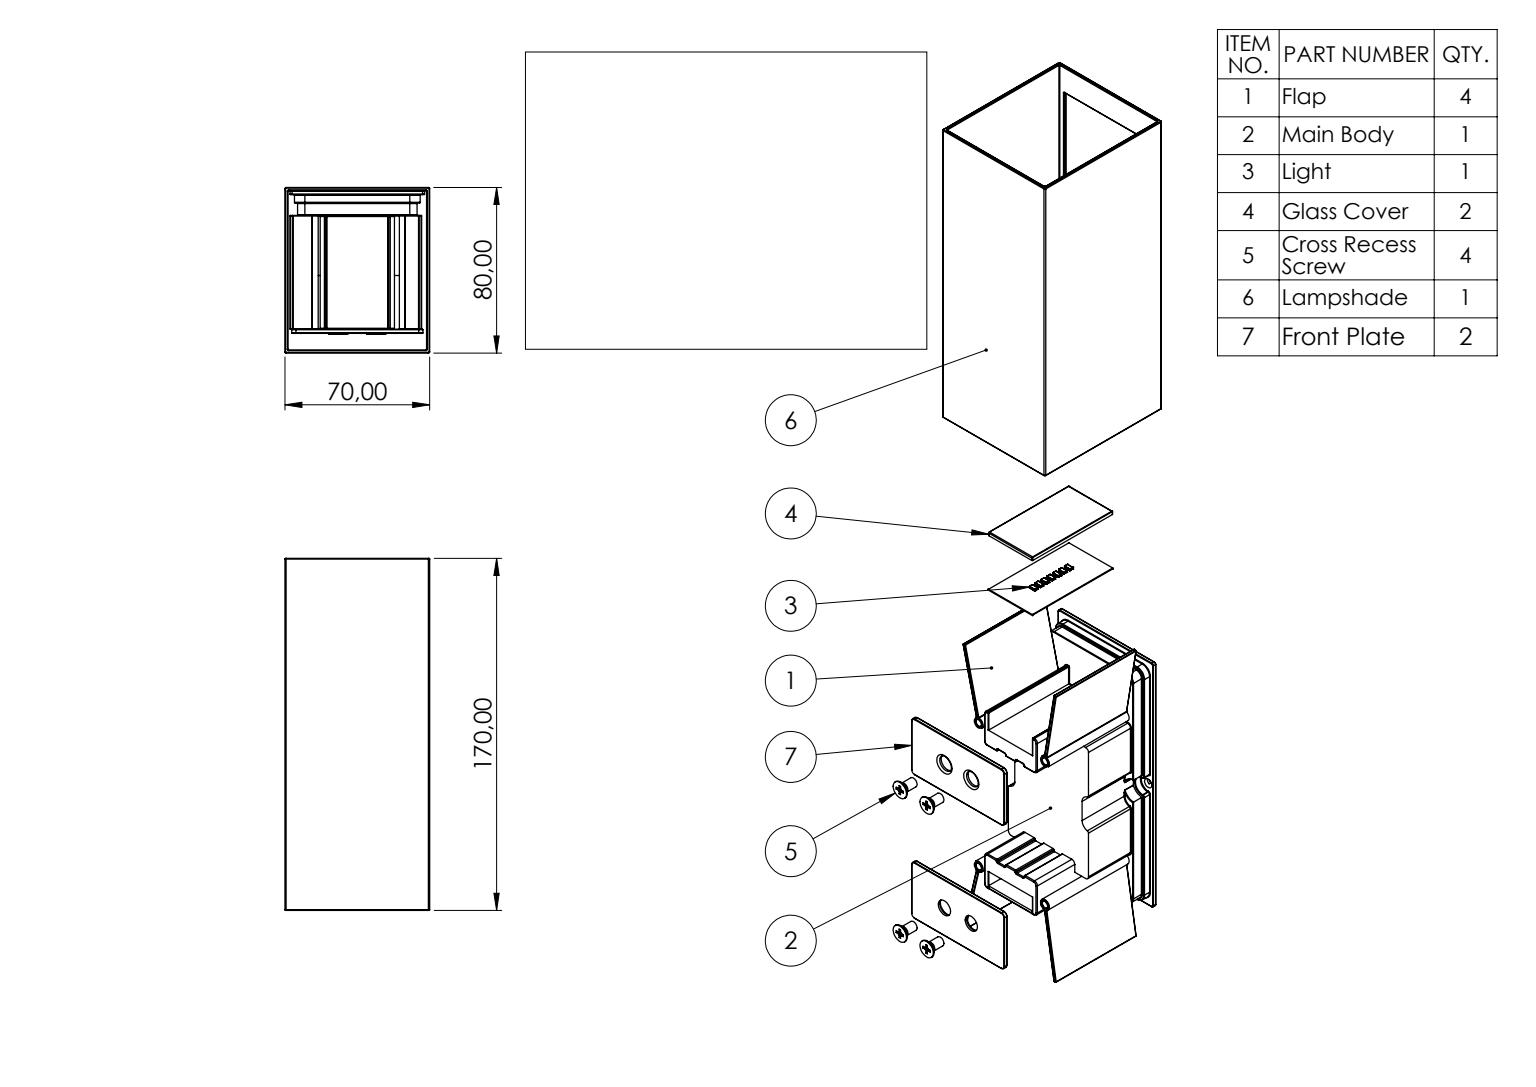
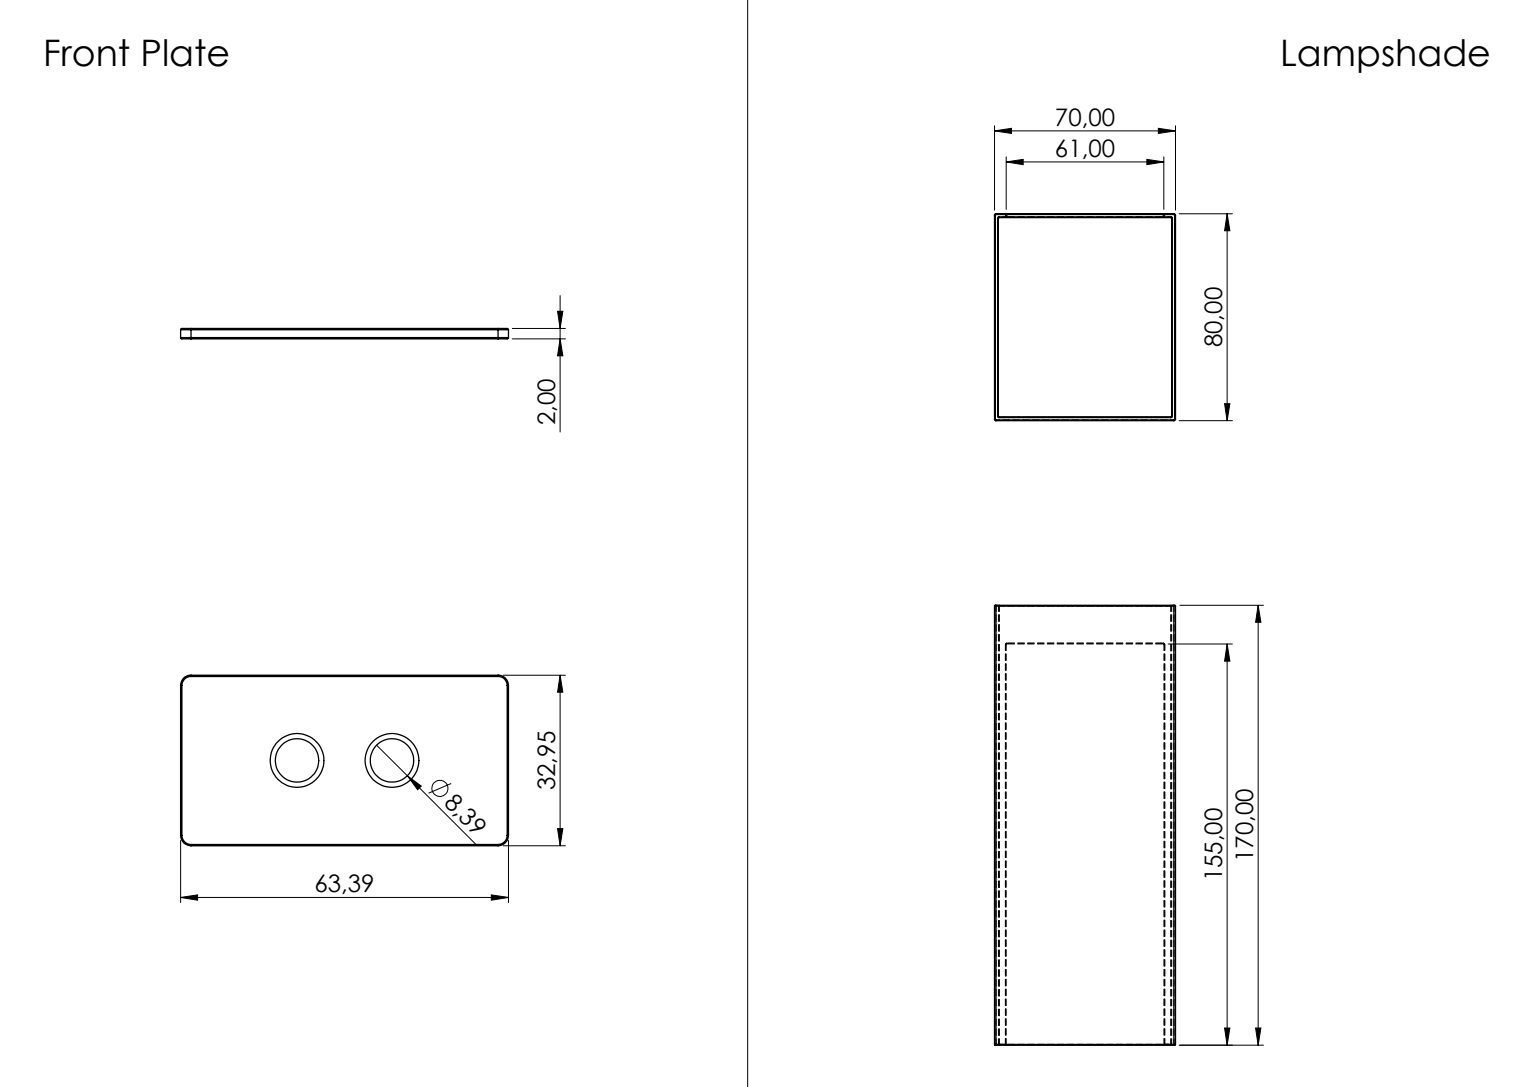
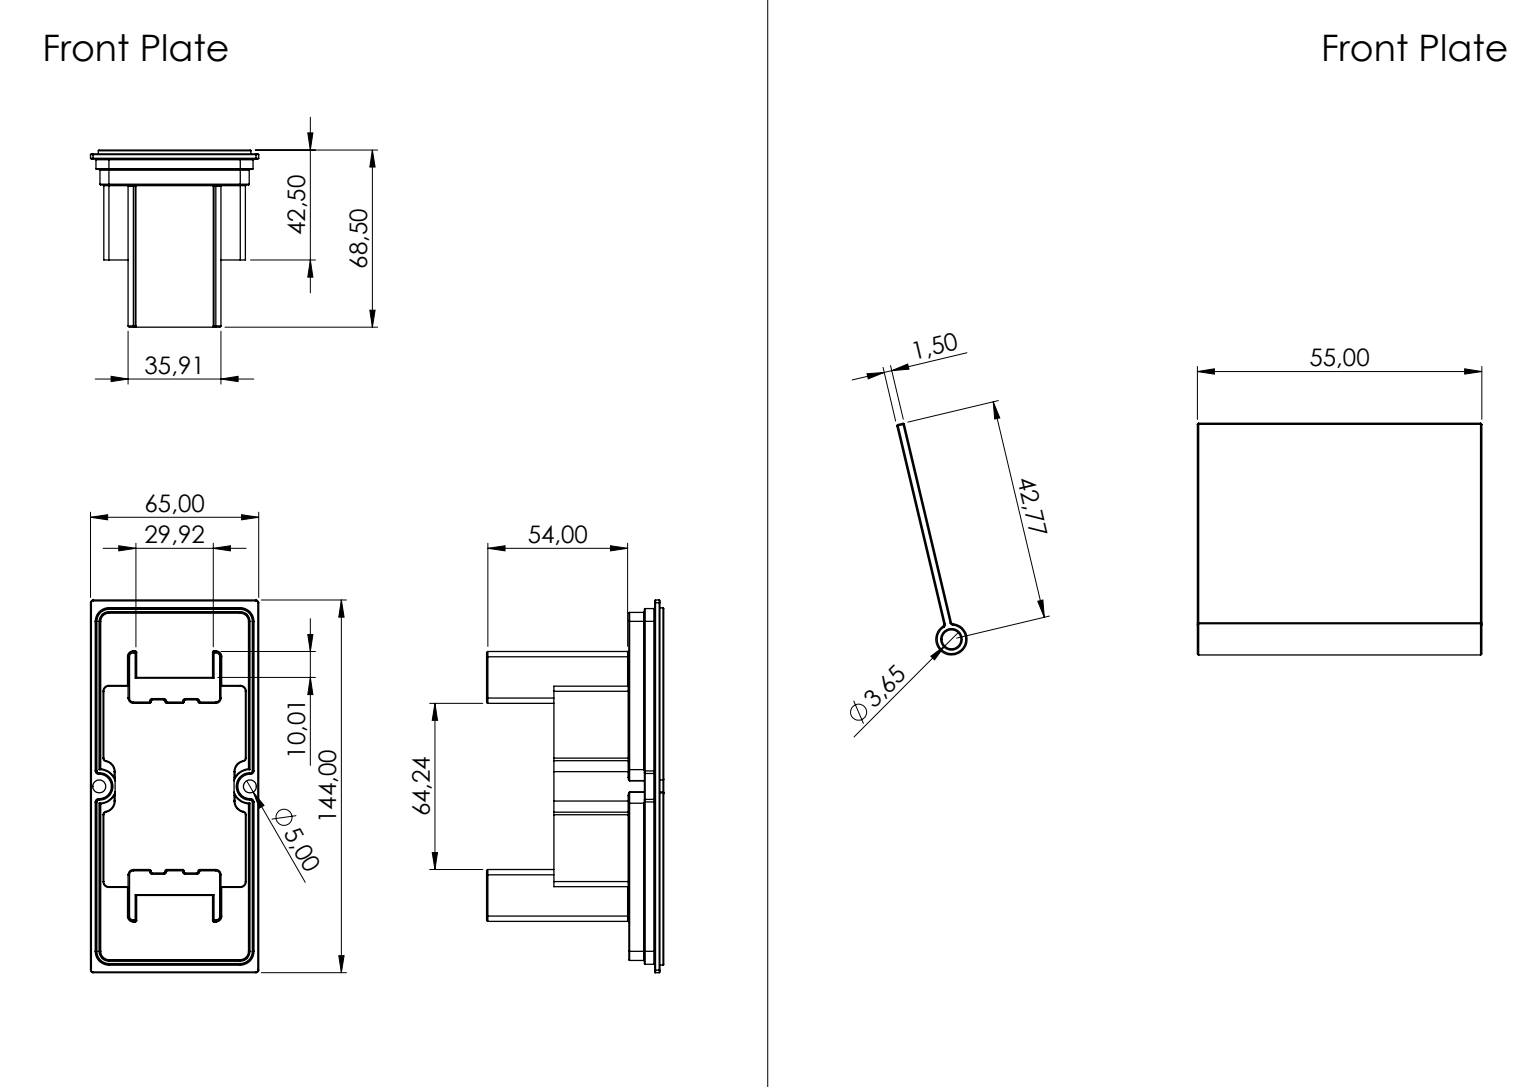
ISO-10303-21;
HEADER;
FILE_DESCRIPTION (('STEP AP214'),
    '1' );
FILE_NAME ('MAS-696',
    '2026-10-07T18:46:32',
    ( '' ),
    ( '' ),
    'SwSTEP 2.0',
    'SolidWorks 2020',
    '' );
FILE_SCHEMA (( 'AUTOMOTIVE_DESIGN' ));
ENDSEC;

DATA;
#1 = DIRECTION ( 'NONE',  ( -1.000000000000000000, 0.000000000000000000, 0.000000000000000000 ) ) ;
#2 = LINE ( 'NONE', #13312, #16468 ) ;
#3 = CARTESIAN_POINT ( 'NONE',  ( -8.638906393579159015, 44.91645089659918710, 70.88527860057354246 ) ) ;
#4 = CARTESIAN_POINT ( 'NONE',  ( -15.21174975910704852, -52.39333383871510108, 13.50000000000000000 ) ) ;
#5 = APPLICATION_CONTEXT ( 'automotive_design' ) ;
#6 = AXIS2_PLACEMENT_3D ( 'NONE', #12347, #7346, #8914 ) ;
#7 = ORIENTED_EDGE ( 'NONE', *, *, #4802, .F. ) ;
#8 = EDGE_CURVE ( 'NONE', #6266, #8265, #9575, .T. ) ;
#9 = CARTESIAN_POINT ( 'NONE',  ( -3.127054932750481964, 33.43424481021354921, 68.00000000000000000 ) ) ;
#10 = DIRECTION ( 'NONE',  ( -1.000000000000000000, 0.000000000000000000, 0.000000000000000000 ) ) ;
#11 = CIRCLE ( 'NONE', #13928, 0.6999999999999992895 ) ;
#12 = CIRCLE ( 'NONE', #12500, 0.2500000000000002220 ) ;
#13 = PRODUCT ( 'MAS-696', 'MAS-696', '', ( #10428 ) ) ;
#14 = CARTESIAN_POINT ( 'NONE',  ( 23.02398829872513986, 5.683640910026983128, 42.50000000000000000 ) ) ;
#15 = EDGE_CURVE ( 'NONE', #14785, #7135, #6042, .T. ) ;
#16 = CARTESIAN_POINT ( 'NONE',  ( 1.724728116533979616, 43.26054587065083012, 27.80876104995653719 ) ) ;
#17 = VERTEX_POINT ( 'NONE', #7499 ) ;
#18 = VERTEX_POINT ( 'NONE', #14070 ) ;
#19 = CARTESIAN_POINT ( 'NONE',  ( 3.127054932750481964, -32.61873716947361856, 68.00000000000000000 ) ) ;
#20 = ORIENTED_EDGE ( 'NONE', *, *, #5140, .T. ) ;
#21 = ORIENTED_EDGE ( 'NONE', *, *, #17514, .T. ) ;
#22 = VERTEX_POINT ( 'NONE', #5719 ) ;
#23 = VECTOR ( 'NONE', #7523, 1000.000000000000000 ) ;
#24 = CYLINDRICAL_SURFACE ( 'NONE', #3799, 0.1000000000000028644 ) ;
#25 = DIRECTION ( 'NONE',  ( 0.000000000000000000, -1.000000000000000000, 0.000000000000000000 ) ) ;
#26 = COLOUR_RGB ( '', 0.09019608, 0.27058824, 0.51372549) ;
#27 = EDGE_CURVE ( 'NONE', #7925, #9580, #2768, .T. ) ;
#28 = CARTESIAN_POINT ( 'NONE',  ( 0.000000000000000000, -51.61873716947361856, 68.50000000000000000 ) ) ;
#29 = DIRECTION ( 'NONE',  ( 0.000000000000000000, 0.000000000000000000, 1.000000000000000000 ) ) ;
#30 = CARTESIAN_POINT ( 'NONE',  ( 14.96174975910705918, 51.61873716947361856, 13.75000000000000000 ) ) ;
#31 = DIRECTION ( 'NONE',  ( 0.000000000000000000, 0.000000000000000000, 1.000000000000000000 ) ) ;
#32 = DIRECTION ( 'NONE',  ( 0.000000000000000000, 0.000000000000000000, 1.000000000000000000 ) ) ;
#33 = CARTESIAN_POINT ( 'NONE',  ( 14.66174975910705314, -51.84675762924568687, 13.49999999999999822 ) ) ;
#34 = EDGE_CURVE ( 'NONE', #6576, #7257, #22097, .T. ) ;
#35 = EDGE_CURVE ( 'NONE', #20423, #10751, #15628, .T. ) ;
#36 = CARTESIAN_POINT ( 'NONE',  ( 29.37540678000427619, 6.000000000000000000, 7.200000000000000178 ) ) ;
#37 = ORIENTED_EDGE ( 'NONE', *, *, #3463, .T. ) ;
#38 = ORIENTED_EDGE ( 'NONE', *, *, #20059, .T. ) ;
#39 = ORIENTED_EDGE ( 'NONE', *, *, #9386, .F. ) ;
#40 = CARTESIAN_POINT ( 'NONE',  ( 0.000000000000000000, -5.299999999999999822, 7.500000000000000000 ) ) ;
#41 = CARTESIAN_POINT ( 'NONE',  ( 25.37540678000427263, 67.24634676501045760, 13.19999999999999929 ) ) ;
#42 = ORIENTED_EDGE ( 'NONE', *, *, #14825, .T. ) ;
#43 = AXIS2_PLACEMENT_3D ( 'NONE', #3141, #11622, #1672 ) ;
#44 = DIRECTION ( 'NONE',  ( 1.000000000000000000, -0.000000000000000000, 0.000000000000000000 ) ) ;
#45 = ADVANCED_BREP_SHAPE_REPRESENTATION ( '', ( #20456, #17493 ), #18569 ) ;
#46 = ORIENTED_EDGE ( 'NONE', *, *, #15265, .F. ) ;
#47 = FACE_OUTER_BOUND ( 'NONE', #3207, .T. ) ;
#48 = DIRECTION ( 'NONE',  ( -1.000000000000000000, 0.000000000000000000, 0.000000000000000000 ) ) ;
#49 = EDGE_CURVE ( 'NONE', #170, #808, #17062, .T. ) ;
#50 = AXIS2_PLACEMENT_3D ( 'NONE', #10111, #15028, #13337 ) ;
#51 = CARTESIAN_POINT ( 'NONE',  ( 15.95292532278785913, 32.11873716947361856, 42.50000000000000711 ) ) ;
#52 = CIRCLE ( 'NONE', #8647, 0.9652499999999990532 ) ;
#53 = EDGE_LOOP ( 'NONE', ( #6761, #19284, #17664, #12954 ) ) ;
#54 = CARTESIAN_POINT ( 'NONE',  ( 25.37540678000427263, -67.24634676501045760, 13.19999999999999929 ) ) ;
#55 = FACE_OUTER_BOUND ( 'NONE', #4259, .T. ) ;
#56 = LINE ( 'NONE', #3411, #9523 ) ;
#57 = CARTESIAN_POINT ( 'NONE',  ( 25.37540678000427263, 63.74634676501045050, 7.200000000000000178 ) ) ;
#58 = DIRECTION ( 'NONE',  ( 1.000000000000000000, 0.000000000000000000, 0.000000000000000000 ) ) ;
#59 = EDGE_LOOP ( 'NONE', ( #5538, #18267, #7700, #20296 ) ) ;
#60 = CYLINDRICAL_SURFACE ( 'NONE', #9129, 0.2999999999999999334 ) ;
#61 = DIRECTION ( 'NONE',  ( -1.000000000000000000, -0.000000000000000000, 0.000000000000000000 ) ) ;
#62 = EDGE_CURVE ( 'NONE', #14667, #2179, #18422, .T. ) ;
#63 = ORIENTED_EDGE ( 'NONE', *, *, #4716, .F. ) ;
#64 = CARTESIAN_POINT ( 'NONE',  ( -30.37540678000427619, 0.000000000000000000, 7.500000000000000000 ) ) ;
#65 = CARTESIAN_POINT ( 'NONE',  ( -8.638906393579159015, 41.66638367286108746, 68.06527860057354928 ) ) ;
#66 = EDGE_CURVE ( 'NONE', #4678, #19429, #10289, .T. ) ;
#67 = DIRECTION ( 'NONE',  ( -1.000000000000000000, 0.000000000000000000, 0.000000000000000000 ) ) ;
#68 = ORIENTED_EDGE ( 'NONE', *, *, #21177, .T. ) ;
#69 = AXIS2_PLACEMENT_3D ( 'NONE', #3279, #6875, #15230 ) ;
#70 = ORIENTED_EDGE ( 'NONE', *, *, #3580, .T. ) ;
#71 = ORIENTED_EDGE ( 'NONE', *, *, #13261, .T. ) ;
#72 = DIRECTION ( 'NONE',  ( 0.000000000000000000, 0.000000000000000000, -1.000000000000000000 ) ) ;
#73 = FACE_OUTER_BOUND ( 'NONE', #20009, .T. ) ;
#74 = AXIS2_PLACEMENT_3D ( 'NONE', #22093, #6650, #20627 ) ;
#75 = CARTESIAN_POINT ( 'NONE',  ( 29.69597781366221767, 58.69165929845684104, 68.50000000000000000 ) ) ;
#76 = VECTOR ( 'NONE', #22096, 1000.000000000000000 ) ;
#77 = ORIENTED_EDGE ( 'NONE', *, *, #5277, .T. ) ;
#78 = ORIENTED_EDGE ( 'NONE', *, *, #20383, .T. ) ;
#79 = CARTESIAN_POINT ( 'NONE',  ( 15.95292532278785913, 34.11873716947361856, 109.6002446535588319 ) ) ;
#80 = ADVANCED_FACE ( 'NONE', ( #2894 ), #13173, .F. ) ;
#81 = ORIENTED_EDGE ( 'NONE', *, *, #14220, .F. ) ;
#82 = DIRECTION ( 'NONE',  ( 0.000000000000000000, 0.000000000000000000, 1.000000000000000000 ) ) ;
#83 = SPHERICAL_SURFACE ( 'NONE', #12076, 0.2500000000000000000 ) ;
#84 = DIRECTION ( 'NONE',  ( -1.224646799147353207E-16, -0.000000000000000000, -1.000000000000000000 ) ) ;
#85 = DIRECTION ( 'NONE',  ( 1.000000000000000000, 0.000000000000000000, 0.000000000000000000 ) ) ;
#86 = ORIENTED_EDGE ( 'NONE', *, *, #5700, .T. ) ;
#87 = CARTESIAN_POINT ( 'NONE',  ( 23.02398829872513986, 3.264788445950721929, 13.78841001078599504 ) ) ;
#88 = LINE ( 'NONE', #10714, #11380 ) ;
#89 = CIRCLE ( 'NONE', #20092, 3.800000000000004707 ) ;
#90 = CIRCLE ( 'NONE', #14366, 0.05000000000000143219 ) ;
#91 = CARTESIAN_POINT ( 'NONE',  ( 0.000000000000000000, 43.26054587065083012, 49.71679706732589921 ) ) ;
#92 = DIRECTION ( 'NONE',  ( 0.000000000000000000, 0.000000000000000000, -1.000000000000000000 ) ) ;
#93 = ORIENTED_EDGE ( 'NONE', *, *, #21253, .F. ) ;
#94 = DIRECTION ( 'NONE',  ( 0.000000000000000000, 0.000000000000000000, -1.000000000000000000 ) ) ;
#95 = ADVANCED_FACE ( 'NONE', ( #9936 ), #19786, .F. ) ;
#96 = EDGE_CURVE ( 'NONE', #20277, #16343, #4681, .T. ) ;
#97 = VERTEX_POINT ( 'NONE', #20017 ) ;
#98 = CIRCLE ( 'NONE', #9390, 0.05000000000000143219 ) ;
#100 = EDGE_CURVE ( 'NONE', #8484, #21526, #21584, .T. ) ;
#99 = CARTESIAN_POINT ( 'NONE',  ( 15.95292532278785913, -50.11873716947361856, 13.79999999999999893 ) ) ;
#101 = LINE ( 'NONE', #6945, #13482 ) ;
#102 = ORIENTED_EDGE ( 'NONE', *, *, #10991, .T. ) ;
#103 = CARTESIAN_POINT ( 'NONE',  ( 1.824728116533979705, 42.36054587065083155, 45.66679706732590205 ) ) ;
#104 = VERTEX_POINT ( 'NONE', #1089 ) ;
#105 = DIRECTION ( 'NONE',  ( -1.000000000000000000, 0.000000000000000000, 0.000000000000000000 ) ) ;
#106 = ORIENTED_EDGE ( 'NONE', *, *, #2093, .F. ) ;
#107 = LINE ( 'NONE', #18791, #3053 ) ;
#108 = LINE ( 'NONE', #1550, #19368 ) ;
#109 = CARTESIAN_POINT ( 'NONE',  ( -17.92752199202934094, 38.74634676501045760, 13.79999999999999893 ) ) ;
#110 = EDGE_CURVE ( 'NONE', #311, #2941, #9931, .T. ) ;
#111 = DIRECTION ( 'NONE',  ( 0.000000000000000000, 0.000000000000000000, 1.000000000000000000 ) ) ;
#112 = CARTESIAN_POINT ( 'NONE',  ( 29.13662752439705272, -5.000000000000000000, 3.799999999999999822 ) ) ;
#113 = FACE_OUTER_BOUND ( 'NONE', #3623, .T. ) ;
#114 = EDGE_CURVE ( 'NONE', #10557, #18072, #13043, .T. ) ;
#115 = ORIENTED_EDGE ( 'NONE', *, *, #9806, .T. ) ;
#116 = FACE_OUTER_BOUND ( 'NONE', #4806, .T. ) ;
#117 = LINE ( 'NONE', #3154, #21755 ) ;
#118 = ORIENTED_EDGE ( 'NONE', *, *, #14708, .F. ) ;
#119 = VERTEX_POINT ( 'NONE', #8152 ) ;
#120 = DIRECTION ( 'NONE',  ( 0.000000000000000000, 1.000000000000000000, 0.000000000000000000 ) ) ;
#121 = ORIENTED_EDGE ( 'NONE', *, *, #13941, .T. ) ;
#122 = PRESENTATION_LAYER_ASSIGNMENT (  '', '', ( #11918 ) ) ;
#123 = ORIENTED_EDGE ( 'NONE', *, *, #13664, .F. ) ;
#124 = VERTEX_POINT ( 'NONE', #8038 ) ;
#125 = EDGE_LOOP ( 'NONE', ( #20790, #19352, #641, #8535 ) ) ;
#126 = EDGE_CURVE ( 'NONE', #6172, #3604, #6011, .T. ) ;
#127 = FACE_OUTER_BOUND ( 'NONE', #20029, .T. ) ;
#128 = LINE ( 'NONE', #15349, #12033 ) ;
#129 = ADVANCED_FACE ( 'NONE', ( #19899 ), #11490, .T. ) ;
#130 = LINE ( 'NONE', #11767, #7823 ) ;
#131 = DIRECTION ( 'NONE',  ( 0.000000000000000000, 0.000000000000000000, -1.000000000000000000 ) ) ;
#132 = CARTESIAN_POINT ( 'NONE',  ( 1.824728116533979261, 43.31054587065082728, 39.80876104995653719 ) ) ;
#133 = DIRECTION ( 'NONE',  ( 0.000000000000000000, 0.000000000000000000, 1.000000000000000000 ) ) ;
#134 = CARTESIAN_POINT ( 'NONE',  ( -30.37540678000427619, -63.74634676501045050, 3.799999999999999822 ) ) ;
#135 = LINE ( 'NONE', #17252, #1789 ) ;
#136 = DIRECTION ( 'NONE',  ( 1.000000000000000000, 0.000000000000000000, 0.000000000000000000 ) ) ;
#137 = ORIENTED_EDGE ( 'NONE', *, *, #1060, .T. ) ;
#138 = ORIENTED_EDGE ( 'NONE', *, *, #854, .T. ) ;
#139 = CARTESIAN_POINT ( 'NONE',  ( 29.13662752439705272, 5.299999999999999822, 7.500000000000000000 ) ) ;
#140 = FACE_OUTER_BOUND ( 'NONE', #8226, .T. ) ;
#141 = CIRCLE ( 'NONE', #1556, 0.04999999999999991257 ) ;
#142 = EDGE_LOOP ( 'NONE', ( #9212, #19592, #9345, #5042 ) ) ;
#143 = EDGE_CURVE ( 'NONE', #15755, #12023, #9721, .T. ) ;
#144 = ADVANCED_FACE ( 'NONE', ( #16287 ), #16748, .F. ) ;
#145 = ORIENTED_EDGE ( 'NONE', *, *, #17677, .T. ) ;
#146 = CARTESIAN_POINT ( 'NONE',  ( -33.50000000000001421, -84.70000000000001705, 78.20000000000000284 ) ) ;
#147 = CIRCLE ( 'NONE', #15855, 1.000000000000000888 ) ;
#148 = CARTESIAN_POINT ( 'NONE',  ( 4.127054932750481520, 33.43424481021354921, 13.50000000000000000 ) ) ;
#149 = EDGE_CURVE ( 'NONE', #13948, #20015, #21002, .T. ) ;
#150 = PLANE ( 'NONE',  #5314 ) ;
#151 = FACE_OUTER_BOUND ( 'NONE', #855, .T. ) ;
#152 = EDGE_LOOP ( 'NONE', ( #5352, #6747, #14198, #4227 ) ) ;
#153 = CARTESIAN_POINT ( 'NONE',  ( 27.37540678000427974, -5.683640910026986681, 13.50000000000000000 ) ) ;
#154 = DIRECTION ( 'NONE',  ( -1.000000000000000000, 0.000000000000000000, -0.000000000000000000 ) ) ;
#155 = DIRECTION ( 'NONE',  ( -0.000000000000000000, 1.000000000000000000, -0.000000000000000000 ) ) ;
#156 = CARTESIAN_POINT ( 'NONE',  ( -21.69312596654449621, 45.47506926072997402, 68.50000000000000000 ) ) ;
#157 = CYLINDRICAL_SURFACE ( 'NONE', #6869, 0.2500000000000002220 ) ;
#158 = DIRECTION ( 'NONE',  ( 1.000000000000000000, 0.000000000000000000, 0.000000000000000000 ) ) ;
#159 = DIRECTION ( 'NONE',  ( 0.000000000000000000, 0.000000000000000000, 1.000000000000000000 ) ) ;
#160 = ORIENTED_EDGE ( 'NONE', *, *, #18200, .F. ) ;
#161 = ORIENTED_EDGE ( 'NONE', *, *, #17115, .T. ) ;
#162 = CIRCLE ( 'NONE', #17316, 2.500000000000002220 ) ;
#163 = ORIENTED_EDGE ( 'NONE', *, *, #4099, .F. ) ;
#164 = CARTESIAN_POINT ( 'NONE',  ( 29.69597781366221767, 58.69165929845684104, 70.50000000000000000 ) ) ;
#165 = EDGE_CURVE ( 'NONE', #17, #1178, #11385, .T. ) ;
#166 = DIRECTION ( 'NONE',  ( 0.000000000000000000, -0.000000000000000000, 1.000000000000000000 ) ) ;
#167 = ORIENTED_EDGE ( 'NONE', *, *, #3663, .F. ) ;
#168 = CARTESIAN_POINT ( 'NONE',  ( -27.37540678000427619, 7.754037881813018962E-15, 42.50000000000000000 ) ) ;
#169 = EDGE_CURVE ( 'NONE', #2258, #13733, #12053, .T. ) ;
#170 = VERTEX_POINT ( 'NONE', #9480 ) ;
#171 = DIRECTION ( 'NONE',  ( -1.224646799147353207E-16, -1.000000000000000000, 0.000000000000000000 ) ) ;
#172 = EDGE_CURVE ( 'NONE', #17257, #3651, #10302, .T. ) ;
#173 = CARTESIAN_POINT ( 'NONE',  ( -1.774728116533986544, 43.26054587065083012, 51.80876104995653719 ) ) ;
#174 = AXIS2_PLACEMENT_3D ( 'NONE', #3147, #1221, #4718 ) ;
#175 = CARTESIAN_POINT ( 'NONE',  ( 30.37540678000427619, 63.74634676501045050, 3.799999999999999822 ) ) ;
#176 = AXIS2_PLACEMENT_3D ( 'NONE', #3775, #19006, #19330 ) ;
#177 = CARTESIAN_POINT ( 'NONE',  ( 33.79999999999999005, 84.70000000000001705, 80.00000000000000000 ) ) ;
#178 = ORIENTED_EDGE ( 'NONE', *, *, #14383, .T. ) ;
#179 = CARTESIAN_POINT ( 'NONE',  ( 23.02398829872513986, 3.528912754968628551, 13.50000000000000178 ) ) ;
#180 = CARTESIAN_POINT ( 'NONE',  ( -30.79999999999999361, -84.70000000000001705, 1.200000000000000400 ) ) ;
#181 = DIRECTION ( 'NONE',  ( -1.788744114411106313E-17, -1.000000000000000000, -1.095289877103613968E-33 ) ) ;
#182 = FACE_OUTER_BOUND ( 'NONE', #18592, .T. ) ;
#183 = VERTEX_POINT ( 'NONE', #20371 ) ;
#184 = CARTESIAN_POINT ( 'NONE',  ( 33.19999999999999574, -84.70000000000001705, 78.20000000000000284 ) ) ;
#185 = ORIENTED_EDGE ( 'NONE', *, *, #2410, .T. ) ;
#186 = VECTOR ( 'NONE', #8638, 1000.000000000000000 ) ;
#187 = LINE ( 'NONE', #20697, #3538 ) ;
#188 = ADVANCED_FACE ( 'NONE', ( #6511 ), #8182, .T. ) ;
#189 = DIRECTION ( 'NONE',  ( 1.000000000000000000, 0.000000000000000000, 0.000000000000000000 ) ) ;
#190 = CIRCLE ( 'NONE', #5215, 2.881677036926254765 ) ;
#191 = EDGE_LOOP ( 'NONE', ( #16439, #11802, #15937, #11017 ) ) ;
#192 = AXIS2_PLACEMENT_3D ( 'NONE', #22000, #16603, #1740 ) ;
#193 = VECTOR ( 'NONE', #20461, 1000.000000000000000 ) ;
#194 = EDGE_LOOP ( 'NONE', ( #10664, #7894, #6707, #20696 ) ) ;
#195 = EDGE_CURVE ( 'NONE', #11031, #19749, #18677, .T. ) ;
#196 = ORIENTED_EDGE ( 'NONE', *, *, #19615, .T. ) ;
#197 = DIRECTION ( 'NONE',  ( 1.000000000000000000, 0.000000000000000000, 0.000000000000000000 ) ) ;
#198 = EDGE_CURVE ( 'NONE', #14667, #21935, #6366, .T. ) ;
#199 = VECTOR ( 'NONE', #1261, 1000.000000000000000 ) ;
#200 = CIRCLE ( 'NONE', #4864, 1.750000000000001554 ) ;
#201 = DIRECTION ( 'NONE',  ( 1.000000000000000000, 0.000000000000000000, -1.224646799147353207E-16 ) ) ;
#202 = EDGE_CURVE ( 'NONE', #5684, #19227, #3019, .T. ) ;
#203 = CARTESIAN_POINT ( 'NONE',  ( 1.724728116533979616, 43.31054587065082728, 39.75876104995653293 ) ) ;
#204 = PRODUCT_DEFINITION_CONTEXT ( 'detailed design', #5, 'design' ) ;
#205 = CARTESIAN_POINT ( 'NONE',  ( -31.26086011588028057, 83.95073979834609190, 68.50000000000000000 ) ) ;
#206 = CIRCLE ( 'NONE', #1997, 0.05000000000000143219 ) ;
#207 = VECTOR ( 'NONE', #21201, 1000.000000000000000 ) ;
#208 = CARTESIAN_POINT ( 'NONE',  ( -4.603906393579157097, 42.46645089659918426, 70.38908280829822672 ) ) ;
#209 = DIRECTION ( 'NONE',  ( -0.000000000000000000, 0.000000000000000000, 1.000000000000000000 ) ) ;
#210 = ORIENTED_EDGE ( 'NONE', *, *, #17092, .T. ) ;
#211 = EDGE_CURVE ( 'NONE', #1488, #12157, #8148, .T. ) ;
#212 = FACE_OUTER_BOUND ( 'NONE', #3377, .T. ) ;
#213 = DIRECTION ( 'NONE',  ( -1.000000000000000000, 0.000000000000000000, 0.000000000000000000 ) ) ;
#215 = DIRECTION ( 'NONE',  ( 0.000000000000000000, 0.000000000000000000, -1.000000000000000000 ) ) ;
#214 = AXIS2_PLACEMENT_3D ( 'NONE', #8138, #16842, #6580 ) ;
#216 = ORIENTED_EDGE ( 'NONE', *, *, #18835, .T. ) ;
#217 = TOROIDAL_SURFACE ( 'NONE', #5616, 0.05000000000000000278, 0.05000000000000000278 ) ;
#218 = ORIENTED_EDGE ( 'NONE', *, *, #9806, .F. ) ;
#219 = DIRECTION ( 'NONE',  ( 0.000000000000000000, 0.000000000000000000, -1.000000000000000000 ) ) ;
#220 = EDGE_LOOP ( 'NONE', ( #1787, #8382, #3209, #12139 ) ) ;
#221 = VECTOR ( 'NONE', #7639, 1000.000000000000000 ) ;
#222 = CARTESIAN_POINT ( 'NONE',  ( 23.02398829872514341, -2.157133568460918305, 13.19999999999998685 ) ) ;
#223 = ORIENTED_EDGE ( 'NONE', *, *, #5319, .F. ) ;
#224 = EDGE_CURVE ( 'NONE', #11867, #21299, #18788, .T. ) ;
#225 = VERTEX_POINT ( 'NONE', #16772 ) ;
#226 = EDGE_CURVE ( 'NONE', #1902, #8285, #10076, .T. ) ;
#227 = CYLINDRICAL_SURFACE ( 'NONE', #2701, 0.2999999999999999334 ) ;
#228 = CARTESIAN_POINT ( 'NONE',  ( -1.724728116533986721, 43.31054587065082728, 51.75876104995654003 ) ) ;
#229 = FACE_OUTER_BOUND ( 'NONE', #21241, .T. ) ;
#230 = CIRCLE ( 'NONE', #5974, 0.2500000000000002220 ) ;
#231 = CIRCLE ( 'NONE', #12723, 0.04999999999999991257 ) ;
#232 = AXIS2_PLACEMENT_3D ( 'NONE', #13801, #5673, #5445 ) ;
#233 = CARTESIAN_POINT ( 'NONE',  ( -25.37540678000427263, 63.74634676501045050, 7.500000000000000000 ) ) ;
#234 = SURFACE_STYLE_USAGE ( .BOTH. , #3717 ) ;
#235 = VECTOR ( 'NONE', #19682, 1000.000000000000000 ) ;
#236 = CARTESIAN_POINT ( 'NONE',  ( 1.724728116533979838, 42.36054587065083155, 33.66679706732590915 ) ) ;
#237 = DIRECTION ( 'NONE',  ( -1.000000000000000000, -0.000000000000000000, -4.336808689942194441E-15 ) ) ;
#238 = CARTESIAN_POINT ( 'NONE',  ( 23.05541308335691042, -2.330322924046650535, 13.28711303755810214 ) ) ;
#239 = DIRECTION ( 'NONE',  ( -1.000000000000000000, -0.000000000000000000, -0.000000000000000000 ) ) ;
#240 = VECTOR ( 'NONE', #10804, 1000.000000000000000 ) ;
#241 = DIRECTION ( 'NONE',  ( 0.000000000000000000, 0.000000000000000000, 1.000000000000000000 ) ) ;
#242 = ORIENTED_EDGE ( 'NONE', *, *, #2603, .F. ) ;
#243 = ORIENTED_EDGE ( 'NONE', *, *, #4452, .F. ) ;
#244 = DIRECTION ( 'NONE',  ( 1.000000000000000000, 0.000000000000000000, 0.000000000000000000 ) ) ;
#245 =( LENGTH_UNIT ( ) NAMED_UNIT ( * ) SI_UNIT ( .MILLI., .METRE. ) );
#247 = EDGE_CURVE ( 'NONE', #13036, #14518, #16350, .T. ) ;
#246 = CARTESIAN_POINT ( 'NONE',  ( -9.141460742840918030, 32.61873716947361856, 68.00000000000000000 ) ) ;
#248 = EDGE_LOOP ( 'NONE', ( #16951, #8078, #4613, #17088 ) ) ;
#249 = AXIS2_PLACEMENT_3D ( 'NONE', #11645, #25, #6874 ) ;
#250 = EDGE_CURVE ( 'NONE', #1621, #2258, #12761, .T. ) ;
#251 = VECTOR ( 'NONE', #6061, 1000.000000000000000 ) ;
#252 = VERTEX_POINT ( 'NONE', #14865 ) ;
#253 = CIRCLE ( 'NONE', #18482, 0.04999999999999991257 ) ;
#254 = AXIS2_PLACEMENT_3D ( 'NONE', #1378, #3292, #10118 ) ;
#255 = DIRECTION ( 'NONE',  ( 1.000000000000000000, 0.000000000000000000, 0.000000000000000000 ) ) ;
#256 = DIRECTION ( 'NONE',  ( 0.000000000000000000, 0.000000000000000000, 1.000000000000000000 ) ) ;
#257 = LINE ( 'NONE', #20968, #15223 ) ;
#258 = VERTEX_POINT ( 'NONE', #1547 ) ;
#259 = DIRECTION ( 'NONE',  ( 0.000000000000000000, 0.000000000000000000, 1.000000000000000000 ) ) ;
#260 = DIRECTION ( 'NONE',  ( 0.000000000000000000, 1.000000000000000000, 0.000000000000000000 ) ) ;
#261 = DIRECTION ( 'NONE',  ( 0.000000000000000000, 0.000000000000000000, 1.000000000000000000 ) ) ;
#262 = CARTESIAN_POINT ( 'NONE',  ( -29.50000000000002132, 2.473451120191013430, 0.2999999999999947153 ) ) ;
#263 = FILL_AREA_STYLE_COLOUR ( '', #16882 ) ;
#264 = CLOSED_SHELL ( 'NONE', ( #4139, #16179, #15323, #8693, #14959, #1658, #17591, #6091, #17555, #5561, #13125, #9357, #12865, #10102, #11748, #5840, #20555, #6272 ) ) ;
#265 = VECTOR ( 'NONE', #8153, 1000.000000000000000 ) ;
#266 = CIRCLE ( 'NONE', #7796, 0.5000000000000004441 ) ;
#267 = CARTESIAN_POINT ( 'NONE',  ( 8.641460742840918030, -33.93424481021354921, 68.50000000000000000 ) ) ;
#268 = EDGE_LOOP ( 'NONE', ( #16094, #16166, #21081, #17689 ) ) ;
#269 = FACE_OUTER_BOUND ( 'NONE', #4169, .T. ) ;
#270 = AXIS2_PLACEMENT_3D ( 'NONE', #2660, #4352, #7834 ) ;
#271 = LINE ( 'NONE', #10799, #1678 ) ;
#272 = ORIENTED_EDGE ( 'NONE', *, *, #425, .T. ) ;
#273 = EDGE_LOOP ( 'NONE', ( #3759, #6135, #19507, #342 ) ) ;
#274 = AXIS2_PLACEMENT_3D ( 'NONE', #12872, #19723, #18021 ) ;
#275 = EDGE_LOOP ( 'NONE', ( #21466, #6868, #2704, #15839 ) ) ;
#276 = CARTESIAN_POINT ( 'NONE',  ( -30.37540678000427619, 63.74634676501045050, 7.200000000000000178 ) ) ;
#277 = PLANE ( 'NONE',  #2427 ) ;
#278 = VECTOR ( 'NONE', #5451, 1000.000000000000000 ) ;
#279 = DIRECTION ( 'NONE',  ( 0.000000000000000000, 0.000000000000000000, -1.000000000000000000 ) ) ;
#280 = EDGE_CURVE ( 'NONE', #2743, #17175, #7794, .T. ) ;
#281 = FACE_OUTER_BOUND ( 'NONE', #19070, .T. ) ;
#282 = ORIENTED_EDGE ( 'NONE', *, *, #19222, .F. ) ;
#283 = DIRECTION ( 'NONE',  ( -0.000000000000000000, -0.000000000000000000, 1.000000000000000000 ) ) ;
#284 = AXIS2_PLACEMENT_3D ( 'NONE', #21562, #13010, #8123 ) ;
#285 = VECTOR ( 'NONE', #15351, 1000.000000000000000 ) ;
#286 = EDGE_LOOP ( 'NONE', ( #6678, #18938, #13760, #4067 ) ) ;
#287 = CARTESIAN_POINT ( 'NONE',  ( -25.37540678000427263, 67.24634676501045760, 13.19999999999999929 ) ) ;
#288 = LINE ( 'NONE', #18996, #14565 ) ;
#289 = AXIS2_PLACEMENT_3D ( 'NONE', #11717, #6380, #11821 ) ;
#290 = DIRECTION ( 'NONE',  ( -0.000000000000000000, -1.000000000000000000, -0.000000000000000000 ) ) ;
#291 = AXIS2_PLACEMENT_3D ( 'NONE', #3039, #1688, #20501 ) ;
#292 = CARTESIAN_POINT ( 'NONE',  ( -1.724728116533986721, 43.26054587065083012, 27.75876104995654003 ) ) ;
#293 = ORIENTED_EDGE ( 'NONE', *, *, #21149, .F. ) ;
#294 = CARTESIAN_POINT ( 'NONE',  ( 23.02398829872513986, 2.191402100636968608, 13.32997043993373154 ) ) ;
#295 = VECTOR ( 'NONE', #10814, 1000.000000000000000 ) ;
#296 = PLANE ( 'NONE',  #14954 ) ;
#297 = DIRECTION ( 'NONE',  ( -0.000000000000000000, 0.000000000000000000, 1.000000000000000000 ) ) ;
#298 = PLANE ( 'NONE',  #15665 ) ;
#299 = VERTEX_POINT ( 'NONE', #20250 ) ;
#300 = ADVANCED_FACE ( 'NONE', ( #11737 ), #986, .T. ) ;
#301 = ORIENTED_EDGE ( 'NONE', *, *, #4018, .F. ) ;
#302 = DIRECTION ( 'NONE',  ( 0.000000000000000000, 0.000000000000000000, 1.000000000000000000 ) ) ;
#303 = CARTESIAN_POINT ( 'NONE',  ( 27.67540678000428045, 7.839012376739720627E-15, 13.79999999999999893 ) ) ;
#304 = TOROIDAL_SURFACE ( 'NONE', #8184, 5.300000000000004263, 0.2999999999999999889 ) ;
#305 = ORIENTED_EDGE ( 'NONE', *, *, #6948, .F. ) ;
#306 = ORIENTED_EDGE ( 'NONE', *, *, #13681, .T. ) ;
#307 = EDGE_CURVE ( 'NONE', #20337, #8429, #10176, .T. ) ;
#308 = EDGE_CURVE ( 'NONE', #12411, #15111, #14209, .T. ) ;
#309 = DIRECTION ( 'NONE',  ( -1.000000000000000000, -0.000000000000000000, -0.000000000000000000 ) ) ;
#310 = AXIS2_PLACEMENT_3D ( 'NONE', #370, #14021, #12447 ) ;
#311 = VERTEX_POINT ( 'NONE', #13532 ) ;
#312 = CIRCLE ( 'NONE', #1010, 0.1000000000000028644 ) ;
#313 = ORIENTED_EDGE ( 'NONE', *, *, #15004, .T. ) ;
#314 = ORIENTED_EDGE ( 'NONE', *, *, #1733, .T. ) ;
#315 = DIRECTION ( 'NONE',  ( 1.000000000000000000, 0.000000000000000000, 0.000000000000000000 ) ) ;
#316 = DIRECTION ( 'NONE',  ( 0.000000000000000000, 1.000000000000000000, 0.000000000000000000 ) ) ;
#317 = DIRECTION ( 'NONE',  ( 0.000000000000000000, 0.000000000000000000, -1.000000000000000000 ) ) ;
#318 = CARTESIAN_POINT ( 'NONE',  ( -31.69597781366222122, 56.94165929845684815, 70.25000000000000000 ) ) ;
#319 = EDGE_CURVE ( 'NONE', #21684, #19115, #1662, .T. ) ;
#320 = AXIS2_PLACEMENT_3D ( 'NONE', #10464, #1935, #8778 ) ;
#321 = FACE_OUTER_BOUND ( 'NONE', #6015, .T. ) ;
#322 = ORIENTED_EDGE ( 'NONE', *, *, #5171, .T. ) ;
#323 = CARTESIAN_POINT ( 'NONE',  ( -17.92752199202933738, 38.74634676501045760, 13.62426406871192874 ) ) ;
#324 = CIRCLE ( 'NONE', #6070, 0.1000000000000028644 ) ;
#325 = CYLINDRICAL_SURFACE ( 'NONE', #22147, 0.2999999999999999334 ) ;
#326 = CARTESIAN_POINT ( 'NONE',  ( 0.000000000000000000, 51.61873716947361856, 14.00000000000000000 ) ) ;
#327 = ORIENTED_EDGE ( 'NONE', *, *, #5171, .F. ) ;
#328 = EDGE_CURVE ( 'NONE', #620, #12977, #10161, .T. ) ;
#329 = FACE_OUTER_BOUND ( 'NONE', #6292, .T. ) ;
#330 = CARTESIAN_POINT ( 'NONE',  ( -14.66895121610833463, 51.92349730072803027, 13.50000000000000000 ) ) ;
#331 = ADVANCED_FACE ( 'NONE', ( #20484 ), #1785, .F. ) ;
#332 = EDGE_LOOP ( 'NONE', ( #15947, #21417, #21604, #10884 ) ) ;
#333 = ORIENTED_EDGE ( 'NONE', *, *, #12972, .T. ) ;
#334 = DIRECTION ( 'NONE',  ( 0.000000000000000000, 0.000000000000000000, 1.000000000000000000 ) ) ;
#335 = ADVANCED_FACE ( 'NONE', ( #13732 ), #17952, .T. ) ;
#336 = DIRECTION ( 'NONE',  ( -1.000000000000000000, 0.000000000000000000, 0.000000000000000000 ) ) ;
#337 = ORIENTED_EDGE ( 'NONE', *, *, #19898, .F. ) ;
#338 = STYLED_ITEM ( 'NONE', ( #10205 ), #45 ) ;
#339 = TOROIDAL_SURFACE ( 'NONE', #15345, 1.500000000000000000, 0.5000000000000000000 ) ;
#340 = CARTESIAN_POINT ( 'NONE',  ( 23.02398829872513986, -2.501891433835003564, 13.57888791970315445 ) ) ;
#341 = VERTEX_POINT ( 'NONE', #9025 ) ;
#342 = ORIENTED_EDGE ( 'NONE', *, *, #4017, .T. ) ;
#343 = DIRECTION ( 'NONE',  ( -0.000000000000000000, 0.000000000000000000, 1.000000000000000000 ) ) ;
#344 = LINE ( 'NONE', #14214, #9144 ) ;
#345 = EDGE_CURVE ( 'NONE', #6305, #10550, #10954, .T. ) ;
#346 = DIRECTION ( 'NONE',  ( -0.000000000000000000, -1.000000000000000000, -0.000000000000000000 ) ) ;
#347 = DIRECTION ( 'NONE',  ( 0.000000000000000000, 0.000000000000000000, 1.000000000000000000 ) ) ;
#348 = DIRECTION ( 'NONE',  ( 0.000000000000000000, 0.000000000000000000, -1.000000000000000000 ) ) ;
#349 = VECTOR ( 'NONE', #15071, 1000.000000000000000 ) ;
#350 = MECHANICAL_DESIGN_GEOMETRIC_PRESENTATION_REPRESENTATION (  '', ( #1426 ), #19311 ) ;
#351 = FACE_OUTER_BOUND ( 'NONE', #21954, .T. ) ;
#352 = LINE ( 'NONE', #21076, #2928 ) ;
#353 = CARTESIAN_POINT ( 'NONE',  ( -30.19999999999999574, 70.00000000000000000, -1.734723475976807094E-15 ) ) ;
#354 = DIRECTION ( 'NONE',  ( 0.000000000000000000, -0.000000000000000000, -1.000000000000000000 ) ) ;
#355 = LINE ( 'NONE', #19056, #20802 ) ;
#356 = EDGE_CURVE ( 'NONE', #2819, #12212, #20621, .T. ) ;
#357 = EDGE_LOOP ( 'NONE', ( #11362, #10177, #13871 ) ) ;
#358 = ORIENTED_EDGE ( 'NONE', *, *, #14725, .T. ) ;
#359 = CYLINDRICAL_SURFACE ( 'NONE', #18503, 0.2999999999999999334 ) ;
#360 = EDGE_CURVE ( 'NONE', #21866, #13036, #8625, .T. ) ;
#361 = LINE ( 'NONE', #5531, #13170 ) ;
#362 = EDGE_LOOP ( 'NONE', ( #19566, #18335, #18750, #10632, #13457, #9597 ) ) ;
#363 = ORIENTED_EDGE ( 'NONE', *, *, #6744, .T. ) ;
#364 = VECTOR ( 'NONE', #5746, 999.9999999999998863 ) ;
#365 = CIRCLE ( 'NONE', #11086, 0.2500000000000002220 ) ;
#366 = CARTESIAN_POINT ( 'NONE',  ( -1.724728116533986721, 42.36054587065083155, 51.70876104995653577 ) ) ;
#367 = CARTESIAN_POINT ( 'NONE',  ( -1.724728116533986721, 42.36054587065083155, 31.75876104995653648 ) ) ;
#368 = EDGE_LOOP ( 'NONE', ( #20999, #1461, #7336 ) ) ;
#369 = CARTESIAN_POINT ( 'NONE',  ( -35.00000000000000000, 84.70000000000001705, 0.6000000000000033085 ) ) ;
#370 = CARTESIAN_POINT ( 'NONE',  ( 0.000000000000000000, -67.24634676501045760, 13.50000000000000000 ) ) ;
#371 = EDGE_CURVE ( 'NONE', #1033, #17036, #14160, .T. ) ;
#372 = DIRECTION ( 'NONE',  ( 1.000000000000000000, 0.000000000000000000, 0.000000000000000000 ) ) ;
#373 = CARTESIAN_POINT ( 'NONE',  ( -18.22752199202934520, 50.11873716947361856, 13.79999999999999716 ) ) ;
#374 = FACE_OUTER_BOUND ( 'NONE', #3857, .T. ) ;
#375 = CARTESIAN_POINT ( 'NONE',  ( 1.774728116533979660, 42.31054587065082728, 29.66679706732590560 ) ) ;
#376 = ORIENTED_EDGE ( 'NONE', *, *, #12243, .F. ) ;
#377 = CARTESIAN_POINT ( 'NONE',  ( -6.297229356652903398, 42.46645089659918426, 68.75385983073485363 ) ) ;
#378 = AXIS2_PLACEMENT_3D ( 'NONE', #16998, #14999, #20380 ) ;
#379 = CARTESIAN_POINT ( 'NONE',  ( -1.774728116533986766, 42.36054587065083155, 33.66679706732590915 ) ) ;
#380 = CARTESIAN_POINT ( 'NONE',  ( 9.641460742840918030, 32.93424481021354921, 68.00000000000000000 ) ) ;
#381 = VERTEX_POINT ( 'NONE', #14371 ) ;
#382 = EDGE_LOOP ( 'NONE', ( #7646, #514, #20961, #15975, #3152, #9896 ) ) ;
#383 = ORIENTED_EDGE ( 'NONE', *, *, #4666, .T. ) ;
#384 = CARTESIAN_POINT ( 'NONE',  ( 27.77120804565216261, -2.094189496455383548, 0.2207451490129595517 ) ) ;
#385 = CARTESIAN_POINT ( 'NONE',  ( 3.627054932750481964, 32.61873716947361856, 42.50000000000000000 ) ) ;
#386 = EDGE_CURVE ( 'NONE', #4334, #5485, #19645, .T. ) ;
#387 = DIRECTION ( 'NONE',  ( 1.000000000000000000, 0.000000000000000000, 0.000000000000000000 ) ) ;
#388 = DIRECTION ( 'NONE',  ( 0.000000000000000000, 0.000000000000000000, -1.000000000000000000 ) ) ;
#389 = CIRCLE ( 'NONE', #16102, 1.999999999999991340 ) ;
#390 = ORIENTED_EDGE ( 'NONE', *, *, #7630, .F. ) ;
#391 = CYLINDRICAL_SURFACE ( 'NONE', #20736, 1.999999999999991340 ) ;
#392 = ORIENTED_EDGE ( 'NONE', *, *, #14902, .T. ) ;
#393 = DIRECTION ( 'NONE',  ( 1.000000000000000000, 0.000000000000000000, 0.000000000000000000 ) ) ;
#394 = CIRCLE ( 'NONE', #4286, 0.6999999999999992895 ) ;
#395 = DIRECTION ( 'NONE',  ( -1.000000000000000000, 0.000000000000000000, 0.000000000000000000 ) ) ;
#396 = CARTESIAN_POINT ( 'NONE',  ( -14.96174975910705207, 42.31054587065082728, 68.25000000000000000 ) ) ;
#397 = FACE_OUTER_BOUND ( 'NONE', #15118, .T. ) ;
#398 = VERTEX_POINT ( 'NONE', #21223 ) ;
#399 = CARTESIAN_POINT ( 'NONE',  ( -15.95292532278785913, 52.39333383871510108, 13.50000000000000000 ) ) ;
#400 = FACE_OUTER_BOUND ( 'NONE', #3553, .T. ) ;
#401 = EDGE_CURVE ( 'NONE', #12977, #16033, #17843, .T. ) ;
#402 = AXIS2_PLACEMENT_3D ( 'NONE', #9005, #19499, #9104 ) ;
#403 = FACE_OUTER_BOUND ( 'NONE', #18761, .T. ) ;
#404 = DIRECTION ( 'NONE',  ( -1.000000000000000000, 0.000000000000000000, 0.000000000000000000 ) ) ;
#405 = EDGE_LOOP ( 'NONE', ( #18020, #19972, #1126, #15256, #10845, #11379 ) ) ;
#406 = EDGE_CURVE ( 'NONE', #16245, #2755, #5261, .T. ) ;
#407 = FACE_OUTER_BOUND ( 'NONE', #12657, .T. ) ;
#408 = ORIENTED_EDGE ( 'NONE', *, *, #2837, .F. ) ;
#409 = CARTESIAN_POINT ( 'NONE',  ( -14.96174975910705207, -32.10873716947361345, 13.79999999999999893 ) ) ;
#410 = VECTOR ( 'NONE', #12305, 1000.000000000000000 ) ;
#411 = LINE ( 'NONE', #17207, #6330 ) ;
#412 = VERTEX_POINT ( 'NONE', #4202 ) ;
#413 = EDGE_LOOP ( 'NONE', ( #18289, #3109, #20862 ) ) ;
#414 = CARTESIAN_POINT ( 'NONE',  ( -29.13662752439705272, -4.700000000000000178, 3.500000000000000000 ) ) ;
#415 = ORIENTED_EDGE ( 'NONE', *, *, #1690, .T. ) ;
#416 = VERTEX_POINT ( 'NONE', #18911 ) ;
#417 = EDGE_CURVE ( 'NONE', #16486, #17755, #10811, .T. ) ;
#418 = CIRCLE ( 'NONE', #10089, 0.5000000000000004441 ) ;
#419 = APPLICATION_CONTEXT ( 'automotive_design' ) ;
#420 = AXIS2_PLACEMENT_3D ( 'NONE', #6413, #21282, #4484 ) ;
#421 = VERTEX_POINT ( 'NONE', #14147 ) ;
#422 = AXIS2_PLACEMENT_3D ( 'NONE', #13047, #1095, #7941 ) ;
#423 = CARTESIAN_POINT ( 'NONE',  ( -30.37540678000427619, 6.000000000000000000, 3.799999999999999822 ) ) ;
#424 = CARTESIAN_POINT ( 'NONE',  ( -25.37540678000427263, -63.74634676501045050, 7.799999999999999822 ) ) ;
#425 = EDGE_CURVE ( 'NONE', #5807, #9408, #20997, .T. ) ;
#426 = CYLINDRICAL_SURFACE ( 'NONE', #3836, 0.05000000000000143219 ) ;
#427 = ORIENTED_EDGE ( 'NONE', *, *, #11746, .F. ) ;
#428 = CARTESIAN_POINT ( 'NONE',  ( 29.20000000000002061, 2.848961824869257864, 0.000000000000000000 ) ) ;
#429 = DIRECTION ( 'NONE',  ( 0.000000000000000000, 1.000000000000000000, 0.000000000000000000 ) ) ;
#430 = DIRECTION ( 'NONE',  ( 1.000000000000000000, 0.000000000000000000, 0.000000000000000000 ) ) ;
#431 = EDGE_LOOP ( 'NONE', ( #5881, #13640, #14381, #15711 ) ) ;
#432 = VECTOR ( 'NONE', #2455, 1000.000000000000000 ) ;
#433 = CYLINDRICAL_SURFACE ( 'NONE', #8151, 6.500000000000002665 ) ;
#434 = ORIENTED_EDGE ( 'NONE', *, *, #11188, .F. ) ;
#435 = AXIS2_PLACEMENT_3D ( 'NONE', #3079, #11240, #1276 ) ;
#436 = ORIENTED_EDGE ( 'NONE', *, *, #17311, .F. ) ;
#437 = ORIENTED_EDGE ( 'NONE', *, *, #20643, .F. ) ;
#438 = FACE_OUTER_BOUND ( 'NONE', #20189, .T. ) ;
#439 = EDGE_CURVE ( 'NONE', #13437, #17644, #9172, .T. ) ;
#440 = VERTEX_POINT ( 'NONE', #4316 ) ;
#441 = ORIENTED_EDGE ( 'NONE', *, *, #14416, .T. ) ;
#442 = AXIS2_PLACEMENT_3D ( 'NONE', #12633, #1915, #14875 ) ;
#443 = CARTESIAN_POINT ( 'NONE',  ( 23.02398829872514341, -3.052854503364608618, 13.54964687161601056 ) ) ;
#444 = VERTEX_POINT ( 'NONE', #17730 ) ;
#445 = VERTEX_POINT ( 'NONE', #5264 ) ;
#446 = EDGE_CURVE ( 'NONE', #22135, #12543, #4899, .T. ) ;
#447 = DIRECTION ( 'NONE',  ( 0.000000000000000000, 0.000000000000000000, -1.000000000000000000 ) ) ;
#448 = ADVANCED_FACE ( 'NONE', ( #17522 ), #612, .T. ) ;
#449 = CYLINDRICAL_SURFACE ( 'NONE', #22037, 2.500000000000002220 ) ;
#450 =( LENGTH_UNIT ( ) NAMED_UNIT ( * ) SI_UNIT ( .MILLI., .METRE. ) );
#451 = DIRECTION ( 'NONE',  ( 1.000000000000000000, 0.000000000000000000, 0.000000000000000000 ) ) ;
#452 = ADVANCED_FACE ( 'NONE', ( #21117 ), #7672, .T. ) ;
#453 = SURFACE_STYLE_FILL_AREA ( #20843 ) ;
#454 = CARTESIAN_POINT ( 'NONE',  ( -23.02398829872513986, 2.333487117377073705, 13.47150829744944467 ) ) ;
#455 = CARTESIAN_POINT ( 'NONE',  ( -29.20000000000002061, 2.799282752659324025, 0.000000000000000000 ) ) ;
#456 = CARTESIAN_POINT ( 'NONE',  ( 34.39999999999998437, 84.70000000000001705, 79.70000000000000284 ) ) ;
#457 = FACE_OUTER_BOUND ( 'NONE', #9813, .T. ) ;
#458 = CARTESIAN_POINT ( 'NONE',  ( -14.96174975910694016, -51.80670431852976776, 13.81236938792817348 ) ) ;
#459 = ORIENTED_EDGE ( 'NONE', *, *, #7526, .F. ) ;
#460 = ORIENTED_EDGE ( 'NONE', *, *, #15953, .F. ) ;
#461 = LINE ( 'NONE', #12538, #11715 ) ;
#462 = CARTESIAN_POINT ( 'NONE',  ( 1.724728116533979616, 42.31054587065082728, 41.71679706732590631 ) ) ;
#463 = EDGE_CURVE ( 'NONE', #1639, #4433, #17022, .T. ) ;
#464 = ORIENTED_EDGE ( 'NONE', *, *, #4413, .T. ) ;
#465 = ORIENTED_EDGE ( 'NONE', *, *, #17617, .T. ) ;
#466 = EDGE_CURVE ( 'NONE', #4617, #17770, #11667, .T. ) ;
#467 = CARTESIAN_POINT ( 'NONE',  ( -1.824728116533986810, 43.31054587065082728, 33.76679706732591058 ) ) ;
#468 = ADVANCED_FACE ( 'NONE', ( #12798 ), #6120, .T. ) ;
#469 = MECHANICAL_DESIGN_GEOMETRIC_PRESENTATION_REPRESENTATION (  '', ( #7640 ), #17639 ) ;
#470 = LINE ( 'NONE', #9099, #3807 ) ;
#471 = VERTEX_POINT ( 'NONE', #1161 ) ;
#472 = LINE ( 'NONE', #17497, #11782 ) ;
#473 = EDGE_CURVE ( 'NONE', #5001, #15844, #1385, .T. ) ;
#474 = DIRECTION ( 'NONE',  ( -0.000000000000000000, -1.000000000000000000, -0.000000000000000000 ) ) ;
#475 = DIRECTION ( 'NONE',  ( -2.832483164223434527E-16, -1.000000000000000000, -0.000000000000000000 ) ) ;
#476 = DIRECTION ( 'NONE',  ( -0.000000000000000000, 0.000000000000000000, 1.000000000000000000 ) ) ;
#477 = DIRECTION ( 'NONE',  ( 0.000000000000000000, 0.000000000000000000, 1.000000000000000000 ) ) ;
#478 = DIRECTION ( 'NONE',  ( -0.000000000000000000, 0.000000000000000000, 1.000000000000000000 ) ) ;
#479 = AXIS2_PLACEMENT_3D ( 'NONE', #5702, #5473, #17200 ) ;
#480 = DIRECTION ( 'NONE',  ( 0.000000000000000000, 1.000000000000000000, 0.000000000000000000 ) ) ;
#481 = DIRECTION ( 'NONE',  ( 1.000000000000000000, 0.000000000000000000, 0.000000000000000000 ) ) ;
#482 = ORIENTED_EDGE ( 'NONE', *, *, #11769, .F. ) ;
#483 = VERTEX_POINT ( 'NONE', #9903 ) ;
#484 = ORIENTED_EDGE ( 'NONE', *, *, #16147, .T. ) ;
#485 = DIRECTION ( 'NONE',  ( 0.000000000000000000, 0.000000000000000000, 1.000000000000000000 ) ) ;
#486 = CARTESIAN_POINT ( 'NONE',  ( -15.95292532278785913, -50.11873716947361856, 13.79999999999999893 ) ) ;
#487 = EDGE_CURVE ( 'NONE', #17808, #7580, #5613, .T. ) ;
#488 = VERTEX_POINT ( 'NONE', #19755 ) ;
#489 = CIRCLE ( 'NONE', #16201, 0.2999999999999999334 ) ;
#490 = PRODUCT_DEFINITION_FORMATION_WITH_SPECIFIED_SOURCE ( 'ANY', '', #16590, .NOT_KNOWN. ) ;
#491 = CARTESIAN_POINT ( 'NONE',  ( 0.000000000000000000, 0.000000000000000000, 68.50000000000000000 ) ) ;
#492 = AXIS2_PLACEMENT_3D ( 'NONE', #6797, #5101, #10245 ) ;
#493 = EDGE_CURVE ( 'NONE', #9687, #4677, #1266, .T. ) ;
#494 = ORIENTED_EDGE ( 'NONE', *, *, #16304, .F. ) ;
#495 = CARTESIAN_POINT ( 'NONE',  ( -14.71174975910705029, 51.61873716947361856, 68.50000000000000000 ) ) ;
#496 = CARTESIAN_POINT ( 'NONE',  ( -9.178906393579158163, 42.46645089659918426, 74.06027860057353962 ) ) ;
#497 = VERTEX_POINT ( 'NONE', #9793 ) ;
#498 = LINE ( 'NONE', #17731, #18144 ) ;
#499 = DIRECTION ( 'NONE',  ( -1.000000000000000000, 0.000000000000000000, 0.000000000000000000 ) ) ;
#500 = CARTESIAN_POINT ( 'NONE',  ( 0.000000000000000000, 66.94634676501046044, 13.19999999999999929 ) ) ;
#501 = LINE ( 'NONE', #14375, #6304 ) ;
#502 = EDGE_LOOP ( 'NONE', ( #20106, #3281, #5812, #15625 ) ) ;
#503 = FACE_OUTER_BOUND ( 'NONE', #10295, .T. ) ;
#504 = EDGE_CURVE ( 'NONE', #14858, #20195, #8459, .T. ) ;
#505 = CARTESIAN_POINT ( 'NONE',  ( 15.95292532278785913, 32.61873716947361856, 68.50000000000000000 ) ) ;
#506 = CYLINDRICAL_SURFACE ( 'NONE', #10149, 1.000000000000000888 ) ;
#507 = ORIENTED_EDGE ( 'NONE', *, *, #21987, .T. ) ;
#508 = DIRECTION ( 'NONE',  ( -1.000000000000000000, 0.000000000000000000, 0.000000000000000000 ) ) ;
#509 = AXIS2_PLACEMENT_3D ( 'NONE', #15002, #3029, #1454 ) ;
#510 = ORIENTED_EDGE ( 'NONE', *, *, #2837, .T. ) ;
#511 = DIRECTION ( 'NONE',  ( -1.000000000000000000, 0.000000000000000000, -0.000000000000000000 ) ) ;
#512 = CARTESIAN_POINT ( 'NONE',  ( -29.37540678000427619, 5.000000000000000000, 7.500000000000000000 ) ) ;
#513 = VERTEX_POINT ( 'NONE', #14925 ) ;
#514 = ORIENTED_EDGE ( 'NONE', *, *, #7199, .T. ) ;
#515 = CARTESIAN_POINT ( 'NONE',  ( -14.96174975910705207, 50.19799549595485644, 68.25000000000000000 ) ) ;
#516 = EDGE_LOOP ( 'NONE', ( #2065, #11314, #11936, #11078 ) ) ;
#517 = EDGE_CURVE ( 'NONE', #5434, #19294, #22048, .T. ) ;
#518 = EDGE_CURVE ( 'NONE', #22136, #10751, #19990, .T. ) ;
#519 = ORIENTED_EDGE ( 'NONE', *, *, #1419, .T. ) ;
#520 = EDGE_CURVE ( 'NONE', #17175, #17812, #16715, .T. ) ;
#521 = VECTOR ( 'NONE', #11856, 1000.000000000000000 ) ;
#522 = STYLED_ITEM ( 'NONE', ( #4431 ), #6179 ) ;
#523 = EDGE_LOOP ( 'NONE', ( #14955, #10482, #2541, #6131 ) ) ;
#524 = DIRECTION ( 'NONE',  ( 1.000000000000000000, -0.000000000000000000, -0.000000000000000000 ) ) ;
#525 = LINE ( 'NONE', #10836, #6531 ) ;
#526 = DIRECTION ( 'NONE',  ( 1.000000000000000000, 0.000000000000000000, 0.000000000000000000 ) ) ;
#527 = ORIENTED_EDGE ( 'NONE', *, *, #6447, .T. ) ;
#528 = CARTESIAN_POINT ( 'NONE',  ( 15.95292532278785913, 50.11873716947361856, 13.79999999999999893 ) ) ;
#529 = AXIS2_PLACEMENT_3D ( 'NONE', #21492, #7709, #12948 ) ;
#530 = CARTESIAN_POINT ( 'NONE',  ( -15.95292532278785913, -50.11873716947361856, 13.87499999999999822 ) ) ;
#531 = LINE ( 'NONE', #10629, #18304 ) ;
#532 = PRODUCT_RELATED_PRODUCT_CATEGORY ( 'part', '', ( #15181 ) ) ;
#533 = EDGE_CURVE ( 'NONE', #10557, #21635, #12019, .T. ) ;
#534 = AXIS2_PLACEMENT_3D ( 'NONE', #11478, #21575, #19882 ) ;
#535 = VECTOR ( 'NONE', #9552, 1000.000000000000000 ) ;
#536 = ORIENTED_EDGE ( 'NONE', *, *, #2118, .T. ) ;
#537 = CARTESIAN_POINT ( 'NONE',  ( -30.19999999999999574, 69.70000000000001705, 1.199999999999999734 ) ) ;
#538 = VERTEX_POINT ( 'NONE', #2738 ) ;
#539 = B_SPLINE_CURVE_WITH_KNOTS ( 'NONE', 3,
 ( #19419, #21120, #4092, #10588, #15827, #20784, #10909, #10708 ),
 .UNSPECIFIED., .F., .F.,
 ( 4, 2, 2, 4 ),
 ( -3.470042892451968281E-06, 0.0002769752510348927397, 0.0004171978979985645165, 0.0005574205449622362391 ),
 .UNSPECIFIED. ) ;
#540 = ORIENTED_EDGE ( 'NONE', *, *, #20299, .T. ) ;
#541 = DIRECTION ( 'NONE',  ( -1.000000000000000000, 0.000000000000000000, 0.000000000000000000 ) ) ;
#542 = CONTEXT_DEPENDENT_SHAPE_REPRESENTATION ( #13717, #13395 ) ;
#543 = EDGE_CURVE ( 'NONE', #13226, #4673, #15590, .T. ) ;
#544 = EDGE_LOOP ( 'NONE', ( #7983, #2781, #18837, #18061 ) ) ;
#545 = ORIENTED_EDGE ( 'NONE', *, *, #13531, .F. ) ;
#546 = EDGE_CURVE ( 'NONE', #19227, #9288, #2374, .T. ) ;
#547 = CIRCLE ( 'NONE', #22014, 0.05000000000000143219 ) ;
#548 = DIRECTION ( 'NONE',  ( 1.000000000000000000, 0.000000000000000000, 0.000000000000000000 ) ) ;
#549 = ORIENTED_EDGE ( 'NONE', *, *, #19963, .F. ) ;
#550 = DIRECTION ( 'NONE',  ( 0.000000000000000000, 0.000000000000000000, 1.000000000000000000 ) ) ;
#551 = AXIS2_PLACEMENT_3D ( 'NONE', #18040, #2721, #16137 ) ;
#552 = AXIS2_PLACEMENT_3D ( 'NONE', #2168, #5667, #18862 ) ;
#553 = AXIS2_PLACEMENT_3D ( 'NONE', #13252, #944, #14600 ) ;
#554 = ORIENTED_EDGE ( 'NONE', *, *, #18237, .T. ) ;
#555 = CARTESIAN_POINT ( 'NONE',  ( -1.836970198721042383E-17, 85.00000000000000000, 0.3000000000000021538 ) ) ;
#556 = CYLINDRICAL_SURFACE ( 'NONE', #14490, 0.5000000000000004441 ) ;
#557 = DIRECTION ( 'NONE',  ( 1.000000000000000000, 0.000000000000000000, 0.000000000000000000 ) ) ;
#558 = DIRECTION ( 'NONE',  ( 0.000000000000000000, 0.000000000000000000, 1.000000000000000000 ) ) ;
#559 = CARTESIAN_POINT ( 'NONE',  ( -25.37540678000427263, 66.94634676501046044, 13.19999999999999929 ) ) ;
#560 = CARTESIAN_POINT ( 'NONE',  ( -33.20000000000000284, 84.70000000000001705, 1.800000000000000266 ) ) ;
#561 = SHAPE_REPRESENTATION ( 'MAS-696', ( #8372, #18343, #14403, #5150, #13338, #16188, #6586, #19068, #18357, #1918, #10870, #20158, #6602, #3003, #1209, #8730 ), #6953 ) ;
#562 = DIRECTION ( 'NONE',  ( 1.000000000000000000, 0.000000000000000000, 0.000000000000000000 ) ) ;
#563 = DIRECTION ( 'NONE',  ( 1.000000000000000000, 0.000000000000000000, 0.000000000000000000 ) ) ;
#564 = AXIS2_PLACEMENT_3D ( 'NONE', #16325, #1004, #14767 ) ;
#565 = VECTOR ( 'NONE', #5582, 1000.000000000000000 ) ;
#566 = ORIENTED_EDGE ( 'NONE', *, *, #11700, .T. ) ;
#567 = VECTOR ( 'NONE', #12317, 1000.000000000000000 ) ;
#568 = EDGE_LOOP ( 'NONE', ( #14082, #870, #8986, #11798 ) ) ;
#569 = LINE ( 'NONE', #7425, #20682 ) ;
#570 = EDGE_CURVE ( 'NONE', #6397, #9425, #13802, .T. ) ;
#571 =( LENGTH_UNIT ( ) NAMED_UNIT ( * ) SI_UNIT ( .MILLI., .METRE. ) );
#572 = EDGE_CURVE ( 'NONE', #13456, #803, #19861, .T. ) ;
#573 = VERTEX_POINT ( 'NONE', #16495 ) ;
#574 = ORIENTED_EDGE ( 'NONE', *, *, #17986, .F. ) ;
#575 = AXIS2_PLACEMENT_3D ( 'NONE', #5688, #15432, #10907 ) ;
#576 = CIRCLE ( 'NONE', #13087, 0.5000000000000004441 ) ;
#577 = CIRCLE ( 'NONE', #9526, 0.05000000000000143219 ) ;
#578 = AXIS2_PLACEMENT_3D ( 'NONE', #18424, #18545, #13175 ) ;
#579 = DIRECTION ( 'NONE',  ( 1.000000000000000000, -0.000000000000000000, 6.123233995736764803E-17 ) ) ;
#580 = B_SPLINE_CURVE_WITH_KNOTS ( 'NONE', 3,
 ( #18832, #1823, #2030, #3723, #8551, #15360, #33, #7097 ),
 .UNSPECIFIED., .F., .F.,
 ( 4, 2, 2, 4 ),
 ( 0.000000000000000000, 0.0004639257417130339422, 0.0006958886125695525667, 0.0009278514834260711370 ),
 .UNSPECIFIED. ) ;
#581 = LINE ( 'NONE', #9211, #6671 ) ;
#582 = CIRCLE ( 'NONE', #10948, 1.000000000000000888 ) ;
#583 = VERTEX_POINT ( 'NONE', #8007 ) ;
#584 = CARTESIAN_POINT ( 'NONE',  ( -22.16013893094044462, 45.60883947780118319, 13.75000000000000000 ) ) ;
#585 = CARTESIAN_POINT ( 'NONE',  ( -24.13662752439704917, 0.000000000000000000, 7.200000000000000178 ) ) ;
#586 = EDGE_CURVE ( 'NONE', #8695, #13748, #1302, .T. ) ;
#587 = DIRECTION ( 'NONE',  ( -1.000000000000000000, 0.000000000000000000, 0.000000000000000000 ) ) ;
#588 = CYLINDRICAL_SURFACE ( 'NONE', #16421, 4.193574995607837863 ) ;
#589 = CARTESIAN_POINT ( 'NONE',  ( -26.63662752439704917, -3.061616997868386099E-16, 0.3000000000000016542 ) ) ;
#590 = DIRECTION ( 'NONE',  ( 0.000000000000000000, -1.000000000000000000, 0.000000000000000000 ) ) ;
#591 = ORIENTED_EDGE ( 'NONE', *, *, #17666, .T. ) ;
#592 = DIRECTION ( 'NONE',  ( 2.832483164223434527E-16, 1.000000000000000000, -0.000000000000000000 ) ) ;
#593 = VECTOR ( 'NONE', #8543, 1000.000000000000000 ) ;
#594 = DIRECTION ( 'NONE',  ( 0.000000000000000000, -1.000000000000000000, 0.000000000000000000 ) ) ;
#595 = EDGE_LOOP ( 'NONE', ( #11628, #11075, #18047, #10530 ) ) ;
#596 = AXIS2_PLACEMENT_3D ( 'NONE', #5143, #1656, #17112 ) ;
#597 = AXIS2_PLACEMENT_3D ( 'NONE', #9978, #8302, #13745 ) ;
#598 = EDGE_LOOP ( 'NONE', ( #10735, #2509, #14989, #19917 ) ) ;
#599 = ORIENTED_EDGE ( 'NONE', *, *, #18143, .F. ) ;
#600 = DIRECTION ( 'NONE',  ( 0.000000000000000000, 0.000000000000000000, -1.000000000000000000 ) ) ;
#601 = EDGE_CURVE ( 'NONE', #10231, #20447, #4653, .T. ) ;
#602 = DIRECTION ( 'NONE',  ( 0.000000000000000000, 0.000000000000000000, -1.000000000000000000 ) ) ;
#603 = ADVANCED_FACE ( 'NONE', ( #20097 ), #16254, .T. ) ;
#604 = VECTOR ( 'NONE', #10624, 1000.000000000000000 ) ;
#605 = ORIENTED_EDGE ( 'NONE', *, *, #2871, .F. ) ;
#606 = EDGE_CURVE ( 'NONE', #8611, #22039, #230, .T. ) ;
#607 = FACE_OUTER_BOUND ( 'NONE', #4232, .T. ) ;
#608 = AXIS2_PLACEMENT_3D ( 'NONE', #14616, #16410, #8029 ) ;
#609 = EDGE_CURVE ( 'NONE', #7850, #7925, #16310, .T. ) ;
#610 = ORIENTED_EDGE ( 'NONE', *, *, #14343, .T. ) ;
#611 = CARTESIAN_POINT ( 'NONE',  ( 0.000000000000000000, 32.61873716947361856, 68.00000000000000000 ) ) ;
#612 = CYLINDRICAL_SURFACE ( 'NONE', #7393, 2.500000000000000444 ) ;
#613 = ORIENTED_EDGE ( 'NONE', *, *, #21858, .F. ) ;
#614 = LINE ( 'NONE', #9243, #11724 ) ;
#615 = PLANE ( 'NONE',  #19962 ) ;
#616 = TOROIDAL_SURFACE ( 'NONE', #20655, 3.750000000000000000, 1.250000000000000000 ) ;
#617 = AXIS2_PLACEMENT_3D ( 'NONE', #8740, #3596, #15537 ) ;
#618 = CARTESIAN_POINT ( 'NONE',  ( 23.02398829872514696, 2.191346223869591991, 13.32987162994455232 ) ) ;
#619 = PLANE ( 'NONE',  #2703 ) ;
#620 = VERTEX_POINT ( 'NONE', #10019 ) ;
#621 = CARTESIAN_POINT ( 'NONE',  ( -18.22752199202934520, -50.11873716947361856, 13.50000000000000000 ) ) ;
#622 = DIRECTION ( 'NONE',  ( 0.000000000000000000, 0.000000000000000000, 1.000000000000000000 ) ) ;
#623 = EDGE_CURVE ( 'NONE', #17862, #9360, #5427, .T. ) ;
#624 = AXIS2_PLACEMENT_3D ( 'NONE', #6692, #5459, #388 ) ;
#625 = DIRECTION ( 'NONE',  ( -0.000000000000000000, 1.000000000000000000, -0.000000000000000000 ) ) ;
#626 = DIRECTION ( 'NONE',  ( 0.000000000000000000, 0.000000000000000000, -1.000000000000000000 ) ) ;
#627 = VERTEX_POINT ( 'NONE', #18964 ) ;
#628 = CIRCLE ( 'NONE', #254, 0.4999999999999995559 ) ;
#629 = AXIS2_PLACEMENT_3D ( 'NONE', #1129, #21630, #6295 ) ;
#630 = VERTEX_POINT ( 'NONE', #21990 ) ;
#631 = DIRECTION ( 'NONE',  ( 0.000000000000000000, 0.000000000000000000, -1.000000000000000000 ) ) ;
#632 = DIRECTION ( 'NONE',  ( -6.123233995736764803E-17, -0.000000000000000000, 1.000000000000000000 ) ) ;
#633 = ORIENTED_EDGE ( 'NONE', *, *, #5654, .T. ) ;
#634 = ORIENTED_EDGE ( 'NONE', *, *, #4459, .T. ) ;
#635 = DIRECTION ( 'NONE',  ( 0.000000000000000000, 0.000000000000000000, 1.000000000000000000 ) ) ;
#636 = CARTESIAN_POINT ( 'NONE',  ( 29.69597781366221767, 56.94165929845684104, 70.25000000000000000 ) ) ;
#637 = EDGE_CURVE ( 'NONE', #19547, #1107, #20309, .T. ) ;
#638 = AXIS2_PLACEMENT_3D ( 'NONE', #14469, #4417, #16496 ) ;
#639 = ORIENTED_EDGE ( 'NONE', *, *, #308, .T. ) ;
#640 = EDGE_CURVE ( 'NONE', #10963, #16873, #16824, .T. ) ;
#641 = ORIENTED_EDGE ( 'NONE', *, *, #21556, .F. ) ;
#642 = CIRCLE ( 'NONE', #5324, 0.04999999999999991257 ) ;
#643 = VECTOR ( 'NONE', #15409, 1000.000000000000000 ) ;
#644 = ORIENTED_EDGE ( 'NONE', *, *, #12918, .T. ) ;
#645 = DIRECTION ( 'NONE',  ( 0.000000000000000000, 1.000000000000000000, 0.000000000000000000 ) ) ;
#646 = DIRECTION ( 'NONE',  ( 0.000000000000000000, 0.000000000000000000, 1.000000000000000000 ) ) ;
#647 = CARTESIAN_POINT ( 'NONE',  ( 4.127054932750481520, -33.93424481021354921, 68.00000000000000000 ) ) ;
#648 = DIRECTION ( 'NONE',  ( 0.000000000000000000, 0.000000000000000000, -1.000000000000000000 ) ) ;
#649 = CARTESIAN_POINT ( 'NONE',  ( 0.000000000000000000, 38.74634676501045760, 42.50000000000000000 ) ) ;
#650 = ORIENTED_EDGE ( 'NONE', *, *, #2014, .T. ) ;
#651 = AXIS2_PLACEMENT_3D ( 'NONE', #13561, #15460, #1364 ) ;
#652 = VECTOR ( 'NONE', #1913, 1000.000000000000000 ) ;
#653 = CARTESIAN_POINT ( 'NONE',  ( 1.824728116533979261, 43.26054587065083012, 31.80876104995653719 ) ) ;
#654 = EDGE_CURVE ( 'NONE', #20195, #15586, #1602, .T. ) ;
#655 = CARTESIAN_POINT ( 'NONE',  ( -29.13662752439705272, 0.000000000000000000, 7.500000000000000000 ) ) ;
#656 = ADVANCED_FACE ( 'NONE', ( #8566 ), #2730, .T. ) ;
#657 = AXIS2_PLACEMENT_3D ( 'NONE', #10919, #19653, #9582 ) ;
#658 = LINE ( 'NONE', #8737, #3312 ) ;
#659 = CIRCLE ( 'NONE', #15255, 0.5999999999999998668 ) ;
#660 = CIRCLE ( 'NONE', #16380, 0.2999999999999999334 ) ;
#661 = ORIENTED_EDGE ( 'NONE', *, *, #701, .F. ) ;
#662 = DIRECTION ( 'NONE',  ( 1.000000000000000000, 0.000000000000000000, 0.000000000000000000 ) ) ;
#663 = ORIENTED_EDGE ( 'NONE', *, *, #13368, .F. ) ;
#664 = EDGE_LOOP ( 'NONE', ( #2962, #17686, #15766, #12256 ) ) ;
#665 = ORIENTED_EDGE ( 'NONE', *, *, #14831, .T. ) ;
#666 = DIRECTION ( 'NONE',  ( 1.000000000000000000, 0.000000000000000000, -0.000000000000000000 ) ) ;
#667 = ADVANCED_FACE ( 'NONE', ( #6666 ), #8444, .T. ) ;
#668 = ORIENTED_EDGE ( 'NONE', *, *, #1242, .F. ) ;
#669 = EDGE_LOOP ( 'NONE', ( #7518, #13127, #6320, #178 ) ) ;
#670 = CIRCLE ( 'NONE', #3550, 0.5000000000000004441 ) ;
#671 = FACE_OUTER_BOUND ( 'NONE', #4656, .T. ) ;
#672 = ORIENTED_EDGE ( 'NONE', *, *, #21439, .F. ) ;
#673 = LINE ( 'NONE', #21274, #6110 ) ;
#674 = AXIS2_PLACEMENT_3D ( 'NONE', #12224, #15382, #1734 ) ;
#675 = VERTEX_POINT ( 'NONE', #12002 ) ;
#676 = VECTOR ( 'NONE', #12838, 1000.000000000000000 ) ;
#677 = FACE_OUTER_BOUND ( 'NONE', #10525, .T. ) ;
#678 = FACE_OUTER_BOUND ( 'NONE', #14910, .T. ) ;
#679 = CARTESIAN_POINT ( 'NONE',  ( 23.32398829872514057, 7.118794219358020148E-15, 13.79999999999999893 ) ) ;
#680 = EDGE_CURVE ( 'NONE', #13756, #9842, #19639, .T. ) ;
#681 = CARTESIAN_POINT ( 'NONE',  ( -23.02398829872514341, 2.681487294389183429, 13.50129116665769757 ) ) ;
#682 = DIRECTION ( 'NONE',  ( 0.000000000000000000, -0.000000000000000000, 1.000000000000000000 ) ) ;
#683 = ADVANCED_FACE ( 'NONE', ( #7274 ), #13214, .T. ) ;
#684 = DIRECTION ( 'NONE',  ( -0.000000000000000000, -1.000000000000000000, -0.000000000000000000 ) ) ;
#685 = CARTESIAN_POINT ( 'NONE',  ( 15.21174975910705918, 42.31054587065082728, 13.50000000000000000 ) ) ;
#686 = CARTESIAN_POINT ( 'NONE',  ( -8.134906293162368129, 43.00645089659919051, 68.06527860057354928 ) ) ;
#687 = AXIS2_PLACEMENT_3D ( 'NONE', #7279, #16083, #20821 ) ;
#688 = ORIENTED_EDGE ( 'NONE', *, *, #10795, .T. ) ;
#689 = VERTEX_POINT ( 'NONE', #5823 ) ;
#690 = ORIENTED_EDGE ( 'NONE', *, *, #5227, .F. ) ;
#691 = ORIENTED_EDGE ( 'NONE', *, *, #15476, .T. ) ;
#692 = ADVANCED_FACE ( 'NONE', ( #4026 ), #7167, .T. ) ;
#693 = CIRCLE ( 'NONE', #3582, 0.2500000000000002220 ) ;
#694 = DIRECTION ( 'NONE',  ( 0.000000000000000000, 0.000000000000000000, -1.000000000000000000 ) ) ;
#695 = TOROIDAL_SURFACE ( 'NONE', #9998, 4.051418481279135619, 0.2999999999999999889 ) ;
#696 = VECTOR ( 'NONE', #15399, 1000.000000000000000 ) ;
#697 = CARTESIAN_POINT ( 'NONE',  ( 30.79999999999999716, -85.00000000000000000, 1.200000000000004174 ) ) ;
#698 = ORIENTED_EDGE ( 'NONE', *, *, #13946, .T. ) ;
#699 = CARTESIAN_POINT ( 'NONE',  ( 3.627054932750481964, 32.93424481021354921, 68.50000000000000000 ) ) ;
#700 = EDGE_CURVE ( 'NONE', #630, #4674, #21089, .T. ) ;
#701 = EDGE_CURVE ( 'NONE', #8457, #13975, #12831, .T. ) ;
#702 = CARTESIAN_POINT ( 'NONE',  ( 18.22752199202934520, -50.11873716947361856, 13.79999999999999716 ) ) ;
#703 = CARTESIAN_POINT ( 'NONE',  ( -29.37540678000427619, -4.700000000000000178, 3.500000000000000000 ) ) ;
#704 = CARTESIAN_POINT ( 'NONE',  ( 15.95292532278785913, -52.11873716947361856, 13.99999999999999822 ) ) ;
#705 = CARTESIAN_POINT ( 'NONE',  ( -23.02398829872513630, 2.192334671524719170, 13.33121981694520741 ) ) ;
#706 = VERTEX_POINT ( 'NONE', #18916 ) ;
#707 = CARTESIAN_POINT ( 'NONE',  ( -25.37540678000427263, 63.74634676501045050, 7.200000000000000178 ) ) ;
#708 = CARTESIAN_POINT ( 'NONE',  ( 1.774728116533979438, 42.36054587065083155, 31.70876104995653932 ) ) ;
#709 = CARTESIAN_POINT ( 'NONE',  ( -8.638906393579159015, 43.26651812033729527, 68.06527860057354928 ) ) ;
#710 = ORIENTED_EDGE ( 'NONE', *, *, #609, .T. ) ;
#711 = ORIENTED_EDGE ( 'NONE', *, *, #13546, .F. ) ;
#712 = VERTEX_POINT ( 'NONE', #3588 ) ;
#713 = DIRECTION ( 'NONE',  ( 1.788744114411106313E-17, 1.000000000000000000, 1.095289877103613968E-33 ) ) ;
#714 = AXIS2_PLACEMENT_3D ( 'NONE', #22113, #11562, #11785 ) ;
#715 = FACE_OUTER_BOUND ( 'NONE', #11040, .T. ) ;
#716 = ORIENTED_EDGE ( 'NONE', *, *, #14040, .T. ) ;
#717 = VECTOR ( 'NONE', #8892, 1000.000000000000000 ) ;
#718 = CARTESIAN_POINT ( 'NONE',  ( -9.178906393579158163, 42.46645089659918426, 68.06527860057354928 ) ) ;
#719 = ADVANCED_FACE ( 'NONE', ( #14628 ), #754, .T. ) ;
#720 = EDGE_LOOP ( 'NONE', ( #6400, #12235, #15309, #196 ) ) ;
#721 = CARTESIAN_POINT ( 'NONE',  ( -1.724728116533986721, 42.36054587065083155, 41.66679706732590915 ) ) ;
#722 = DIRECTION ( 'NONE',  ( 0.000000000000000000, 0.000000000000000000, -1.000000000000000000 ) ) ;
#723 = DIRECTION ( 'NONE',  ( 0.000000000000000000, 0.000000000000000000, 1.000000000000000000 ) ) ;
#724 = DIRECTION ( 'NONE',  ( -0.000000000000000000, -0.000000000000000000, -1.000000000000000000 ) ) ;
#725 = CARTESIAN_POINT ( 'NONE',  ( 29.37540678000427619, 4.700000000000000178, 3.799999999999999822 ) ) ;
#726 = CARTESIAN_POINT ( 'NONE',  ( 23.02398829872513986, 7.027230193580998154E-15, 42.50000000000000000 ) ) ;
#727 = ORIENTED_EDGE ( 'NONE', *, *, #10966, .T. ) ;
#728 = CYLINDRICAL_SURFACE ( 'NONE', #19170, 0.04999999999999991257 ) ;
#729 = DIRECTION ( 'NONE',  ( 1.000000000000000000, -0.000000000000000000, 0.000000000000000000 ) ) ;
#730 = AXIS2_PLACEMENT_3D ( 'NONE', #20003, #12923, #6133 ) ;
#731 = EDGE_CURVE ( 'NONE', #3842, #12280, #19290, .T. ) ;
#732 = AXIS2_PLACEMENT_3D ( 'NONE', #11982, #10438, #13447 ) ;
#733 = EDGE_CURVE ( 'NONE', #13680, #14946, #8024, .T. ) ;
#734 = CYLINDRICAL_SURFACE ( 'NONE', #12273, 0.5000000000000004441 ) ;
#735 = FACE_OUTER_BOUND ( 'NONE', #7826, .T. ) ;
#736 = ORIENTED_EDGE ( 'NONE', *, *, #7228, .F. ) ;
#737 = FILL_AREA_STYLE_COLOUR ( '', #2686 ) ;
#738 = ORIENTED_EDGE ( 'NONE', *, *, #19674, .F. ) ;
#739 = DIRECTION ( 'NONE',  ( 0.000000000000000000, 1.000000000000000000, 0.000000000000000000 ) ) ;
#740 = DIRECTION ( 'NONE',  ( 0.000000000000000000, 0.000000000000000000, -1.000000000000000000 ) ) ;
#741 = ORIENTED_EDGE ( 'NONE', *, *, #19369, .T. ) ;
#742 = EDGE_LOOP ( 'NONE', ( #18223, #13014, #9930, #12285, #20664, #4144, #15061 ) ) ;
#743 = DIRECTION ( 'NONE',  ( 0.000000000000000000, -1.000000000000000000, 0.000000000000000000 ) ) ;
#744 = LINE ( 'NONE', #9713, #19223 ) ;
#745 = DIRECTION ( 'NONE',  ( -0.000000000000000000, -1.000000000000000000, -0.000000000000000000 ) ) ;
#746 = AXIS2_PLACEMENT_3D ( 'NONE', #20659, #18330, #20545 ) ;
#747 = ORIENTED_EDGE ( 'NONE', *, *, #3492, .F. ) ;
#748 = EDGE_CURVE ( 'NONE', #258, #7522, #17875, .T. ) ;
#749 = CIRCLE ( 'NONE', #378, 0.2500000000000002220 ) ;
#750 = EDGE_LOOP ( 'NONE', ( #18594, #12319, #18530, #4136 ) ) ;
#751 = CARTESIAN_POINT ( 'NONE',  ( -18.22752199202934520, 50.11873716947361856, 13.79999999999999716 ) ) ;
#752 = AXIS2_PLACEMENT_3D ( 'NONE', #5771, #14246, #10791 ) ;
#753 = AXIS2_PLACEMENT_3D ( 'NONE', #12913, #9578, #1063 ) ;
#754 = PLANE ( 'NONE',  #8215 ) ;
#755 = CARTESIAN_POINT ( 'NONE',  ( -23.02398829872513986, 2.157133568460765538, 13.19999999999999929 ) ) ;
#756 = CARTESIAN_POINT ( 'NONE',  ( 1.774728116533979438, 42.36054587065083155, 35.70876104995653577 ) ) ;
#757 = EDGE_CURVE ( 'NONE', #4673, #21472, #14282, .T. ) ;
#758 = AXIS2_PLACEMENT_3D ( 'NONE', #11447, #1370, #8103 ) ;
#759 = AXIS2_PLACEMENT_3D ( 'NONE', #4076, #15914, #21102 ) ;
#760 = ADVANCED_FACE ( 'NONE', ( #5920 ), #19446, .T. ) ;
#761 = DIRECTION ( 'NONE',  ( -1.000000000000000000, 0.000000000000000000, 0.000000000000000000 ) ) ;
#762 = DIRECTION ( 'NONE',  ( 0.000000000000000000, 0.000000000000000000, 1.000000000000000000 ) ) ;
#763 = EDGE_LOOP ( 'NONE', ( #11586, #167, #21202, #9598 ) ) ;
#764 = DIRECTION ( 'NONE',  ( -0.000000000000000000, 0.000000000000000000, 1.000000000000000000 ) ) ;
#765 = EDGE_CURVE ( 'NONE', #16245, #21932, #11058, .T. ) ;
#766 = DIRECTION ( 'NONE',  ( -0.000000000000000000, -1.000000000000000000, -0.000000000000000000 ) ) ;
#767 = CARTESIAN_POINT ( 'NONE',  ( -25.37540678000429040, -36.74634676501047181, 42.50000000000000000 ) ) ;
#768 = DIRECTION ( 'NONE',  ( 0.000000000000000000, 0.000000000000000000, 1.000000000000000000 ) ) ;
#769 = FACE_OUTER_BOUND ( 'NONE', #17919, .T. ) ;
#770 = ORIENTED_EDGE ( 'NONE', *, *, #13810, .F. ) ;
#771 = CIRCLE ( 'NONE', #9361, 1.750000000000001554 ) ;
#772 = ORIENTED_EDGE ( 'NONE', *, *, #10656, .F. ) ;
#773 = DIRECTION ( 'NONE',  ( 0.000000000000000000, 0.000000000000000000, 1.000000000000000000 ) ) ;
#774 = CONTEXT_DEPENDENT_SHAPE_REPRESENTATION ( #8437, #20570 ) ;
#775 = EDGE_CURVE ( 'NONE', #21472, #8556, #11055, .T. ) ;
#776 = ORIENTED_EDGE ( 'NONE', *, *, #11838, .T. ) ;
#777 = CIRCLE ( 'NONE', #15079, 0.2999999999999999334 ) ;
#778 = AXIS2_PLACEMENT_3D ( 'NONE', #8553, #15361, #136 ) ;
#779 = ORIENTED_EDGE ( 'NONE', *, *, #1035, .F. ) ;
#780 = VECTOR ( 'NONE', #12733, 1000.000000000000000 ) ;
#781 = EDGE_CURVE ( 'NONE', #7899, #17644, #4648, .T. ) ;
#782 = FACE_OUTER_BOUND ( 'NONE', #16557, .T. ) ;
#783 = ORIENTED_EDGE ( 'NONE', *, *, #6213, .F. ) ;
#784 = CARTESIAN_POINT ( 'NONE',  ( 1.724728116533979838, 43.26054587065083012, 45.66679706732590205 ) ) ;
#785 = EDGE_LOOP ( 'NONE', ( #15704, #12399, #12620, #13658 ) ) ;
#786 = CARTESIAN_POINT ( 'NONE',  ( -1.724728116533986721, 43.31054587065082728, 41.66679706732590915 ) ) ;
#787 = DIRECTION ( 'NONE',  ( 1.000000000000000000, 0.000000000000000000, 0.000000000000000000 ) ) ;
#788 = DIRECTION ( 'NONE',  ( 0.000000000000000000, 0.000000000000000000, 1.000000000000000000 ) ) ;
#789 = CARTESIAN_POINT ( 'NONE',  ( 34.39999999999998437, 84.70000000000001705, 0.6000000000000041966 ) ) ;
#790 = ADVANCED_FACE ( 'NONE', ( #7940 ), #18215, .T. ) ;
#791 = AXIS2_PLACEMENT_3D ( 'NONE', #4461, #16192, #14408 ) ;
#792 = DIRECTION ( 'NONE',  ( 1.000000000000000000, 0.000000000000000000, 0.000000000000000000 ) ) ;
#793 = CIRCLE ( 'NONE', #21886, 0.2999999999999999334 ) ;
#794 = DIRECTION ( 'NONE',  ( 0.000000000000000000, 1.000000000000000000, 0.000000000000000000 ) ) ;
#795 = FACE_OUTER_BOUND ( 'NONE', #2508, .T. ) ;
#796 = DIRECTION ( 'NONE',  ( 0.000000000000000000, -0.000000000000000000, -1.000000000000000000 ) ) ;
#797 = PLANE ( 'NONE',  #6379 ) ;
#798 = ORIENTED_EDGE ( 'NONE', *, *, #518, .F. ) ;
#799 = VERTEX_POINT ( 'NONE', #14842 ) ;
#800 = DIRECTION ( 'NONE',  ( 0.000000000000000000, 0.000000000000000000, -1.000000000000000000 ) ) ;
#801 = AXIS2_PLACEMENT_3D ( 'NONE', #4744, #14793, #5982 ) ;
#802 = CYLINDRICAL_SURFACE ( 'NONE', #15979, 0.05000000000000143219 ) ;
#803 = VERTEX_POINT ( 'NONE', #6154 ) ;
#804 = ADVANCED_FACE ( 'NONE', ( #19679 ), #4350, .T. ) ;
#805 = EDGE_CURVE ( 'NONE', #11236, #19185, #21443, .T. ) ;
#806 = FACE_OUTER_BOUND ( 'NONE', #2034, .T. ) ;
#807 = FACE_OUTER_BOUND ( 'NONE', #742, .T. ) ;
#808 = VERTEX_POINT ( 'NONE', #9483 ) ;
#809 = FACE_BOUND ( 'NONE', #18279, .T. ) ;
#810 = LINE ( 'NONE', #4507, #7614 ) ;
#811 = CARTESIAN_POINT ( 'NONE',  ( -28.57540678000427548, 6.776800961815481195, 13.50000000000000000 ) ) ;
#812 = DIRECTION ( 'NONE',  ( 0.000000000000000000, 0.000000000000000000, 1.000000000000000000 ) ) ;
#813 = DIRECTION ( 'NONE',  ( 1.987703982890080681E-15, 0.000000000000000000, -1.000000000000000000 ) ) ;
#814 = VERTEX_POINT ( 'NONE', #4241 ) ;
#815 = DIRECTION ( 'NONE',  ( -8.673617379884034239E-17, -0.000000000000000000, 1.000000000000000000 ) ) ;
#816 = LINE ( 'NONE', #14454, #15563 ) ;
#817 = CARTESIAN_POINT ( 'NONE',  ( -15.95292532278785913, 50.11873716947361856, 13.79999999999999893 ) ) ;
#818 = VERTEX_POINT ( 'NONE', #2898 ) ;
#819 = ORIENTED_EDGE ( 'NONE', *, *, #2444, .T. ) ;
#820 = ORIENTED_EDGE ( 'NONE', *, *, #20766, .T. ) ;
#821 = DIRECTION ( 'NONE',  ( -1.000000000000000000, -0.000000000000000000, -0.000000000000000000 ) ) ;
#822 = DIRECTION ( 'NONE',  ( 0.000000000000000000, 0.000000000000000000, 1.000000000000000000 ) ) ;
#823 = VERTEX_POINT ( 'NONE', #13046 ) ;
#824 = DIRECTION ( 'NONE',  ( 0.000000000000000000, 0.000000000000000000, 1.000000000000000000 ) ) ;
#825 = EDGE_CURVE ( 'NONE', #3127, #1963, #7517, .T. ) ;
#826 = ORIENTED_EDGE ( 'NONE', *, *, #19386, .T. ) ;
#827 = CARTESIAN_POINT ( 'NONE',  ( -29.37540678000427619, -5.000000000000000000, 7.500000000000000000 ) ) ;
#828 = DIRECTION ( 'NONE',  ( -0.000000000000000000, -1.000000000000000000, -0.000000000000000000 ) ) ;
#829 = CARTESIAN_POINT ( 'NONE',  ( 23.02398829872513630, -2.333754220862764406, 13.47170153661532943 ) ) ;
#830 = DIRECTION ( 'NONE',  ( 0.000000000000000000, 0.000000000000000000, 1.000000000000000000 ) ) ;
#831 = CARTESIAN_POINT ( 'NONE',  ( -1.724728116533986721, 42.36054587065083155, 31.70876104995653932 ) ) ;
#832 = CARTESIAN_POINT ( 'NONE',  ( 1.724728116533979616, 43.26054587065083012, 47.70876104995654288 ) ) ;
#833 = VERTEX_POINT ( 'NONE', #19788 ) ;
#834 = LINE ( 'NONE', #19652, #7743 ) ;
#835 = DIRECTION ( 'NONE',  ( 0.000000000000000000, 0.000000000000000000, -1.000000000000000000 ) ) ;
#836 = CIRCLE ( 'NONE', #13347, 0.2500000000000002220 ) ;
#837 = DIRECTION ( 'NONE',  ( -1.000000000000000000, 0.000000000000000000, 0.000000000000000000 ) ) ;
#838 = CARTESIAN_POINT ( 'NONE',  ( -1.724728116533986721, 43.26054587065083012, 49.66679706732590915 ) ) ;
#839 = ORIENTED_EDGE ( 'NONE', *, *, #12806, .T. ) ;
#840 = CYLINDRICAL_SURFACE ( 'NONE', #19835, 0.3000000000000003775 ) ;
#841 = LINE ( 'NONE', #21347, #8216 ) ;
#842 = EDGE_CURVE ( 'NONE', #17942, #4860, #4449, .T. ) ;
#843 = ORIENTED_EDGE ( 'NONE', *, *, #15926, .F. ) ;
#844 = DIRECTION ( 'NONE',  ( 1.000000000000000000, 0.000000000000000000, 0.000000000000000000 ) ) ;
#845 = AXIS2_PLACEMENT_3D ( 'NONE', #11623, #22060, #18688 ) ;
#846 = DIRECTION ( 'NONE',  ( -1.734723475976806848E-16, 0.000000000000000000, 1.000000000000000000 ) ) ;
#847 = VERTEX_POINT ( 'NONE', #1094 ) ;
#848 = ORIENTED_EDGE ( 'NONE', *, *, #1937, .F. ) ;
#849 = LINE ( 'NONE', #18928, #10964 ) ;
#850 = FACE_OUTER_BOUND ( 'NONE', #16602, .T. ) ;
#851 = PLANE ( 'NONE',  #1729 ) ;
#852 = VERTEX_POINT ( 'NONE', #19905 ) ;
#853 = EDGE_CURVE ( 'NONE', #4495, #3678, #14742, .T. ) ;
#854 = EDGE_CURVE ( 'NONE', #6442, #21823, #693, .T. ) ;
#855 = EDGE_LOOP ( 'NONE', ( #21772, #772, #17828, #9443 ) ) ;
#856 = CARTESIAN_POINT ( 'NONE',  ( -33.20000000000000284, -84.70000000000001705, 1.500000000000000222 ) ) ;
#857 = VERTEX_POINT ( 'NONE', #18322 ) ;
#858 = CARTESIAN_POINT ( 'NONE',  ( -20.58855031337657593, 86.74083381065993592, 68.25000000000000000 ) ) ;
#859 = DIRECTION ( 'NONE',  ( 0.9729678061520320442, 0.2309407893632090536, 0.000000000000000000 ) ) ;
#860 = DIRECTION ( 'NONE',  ( 0.000000000000000000, 0.000000000000000000, 1.000000000000000000 ) ) ;
#861 = CARTESIAN_POINT ( 'NONE',  ( 1.774728116533979660, 43.31054587065082728, 49.66679706732590915 ) ) ;
#862 = CARTESIAN_POINT ( 'NONE',  ( 29.69597781366221767, 26.24124249474150972, 68.50000000000000000 ) ) ;
#863 = EDGE_LOOP ( 'NONE', ( #11456, #18394, #7375, #7367, #8850, #15864, #38, #6946 ) ) ;
#864 = CARTESIAN_POINT ( 'NONE',  ( -32.48382792203229741, 83.71979900898287497, 68.25000000000000000 ) ) ;
#865 = EDGE_CURVE ( 'NONE', #8082, #15018, #16059, .T. ) ;
#866 = DIRECTION ( 'NONE',  ( 0.000000000000000000, 1.000000000000000000, -0.000000000000000000 ) ) ;
#867 = CARTESIAN_POINT ( 'NONE',  ( 9.641460742840918030, -33.43424481021354921, 68.00000000000000000 ) ) ;
#868 = DIRECTION ( 'NONE',  ( 0.000000000000000000, 0.000000000000000000, 1.000000000000000000 ) ) ;
#869 = FACE_BOUND ( 'NONE', #11844, .T. ) ;
#870 = ORIENTED_EDGE ( 'NONE', *, *, #9475, .T. ) ;
#871 = CIRCLE ( 'NONE', #14819, 0.1000000000000028644 ) ;
#872 = EDGE_LOOP ( 'NONE', ( #19202, #1679, #14033, #20667 ) ) ;
#873 = AXIS2_PLACEMENT_3D ( 'NONE', #4273, #7741, #19821 ) ;
#874 = DIRECTION ( 'NONE',  ( -0.000000000000000000, 1.000000000000000000, -0.000000000000000000 ) ) ;
#875 = SHAPE_DEFINITION_REPRESENTATION ( #17162, #3995 ) ;
#876 = EDGE_CURVE ( 'NONE', #7599, #21952, #14988, .T. ) ;
#877 = VERTEX_POINT ( 'NONE', #21812 ) ;
#878 = EDGE_CURVE ( 'NONE', #1886, #11776, #20372, .T. ) ;
#879 = VERTEX_POINT ( 'NONE', #15298 ) ;
#880 = EDGE_CURVE ( 'NONE', #19512, #8125, #12482, .T. ) ;
#881 = ORIENTED_EDGE ( 'NONE', *, *, #7498, .T. ) ;
#882 = DIRECTION ( 'NONE',  ( 0.000000000000000000, -0.000000000000000000, -1.000000000000000000 ) ) ;
#883 = ORIENTED_EDGE ( 'NONE', *, *, #16397, .F. ) ;
#884 = DIRECTION ( 'NONE',  ( 0.000000000000000000, 0.000000000000000000, -1.000000000000000000 ) ) ;
#885 = DIRECTION ( 'NONE',  ( -1.000000000000000000, 0.000000000000000000, 0.000000000000000000 ) ) ;
#886 = CARTESIAN_POINT ( 'NONE',  ( -1.724728116533986721, 42.36054587065083155, 45.71679706732590631 ) ) ;
#887 = AXIS2_PLACEMENT_3D ( 'NONE', #9917, #13697, #8245 ) ;
#888 = AXIS2_PLACEMENT_3D ( 'NONE', #8018, #9255, #14482 ) ;
#889 = CARTESIAN_POINT ( 'NONE',  ( -1.724728116533986721, 43.31054587065082728, 31.70876104995653932 ) ) ;
#890 = ADVANCED_FACE ( 'NONE', ( #16862 ), #6705, .F. ) ;
#891 = DIRECTION ( 'NONE',  ( -1.000000000000000000, 0.000000000000000000, 0.000000000000000000 ) ) ;
#892 = CARTESIAN_POINT ( 'NONE',  ( 1.774728116533973665, 43.26054587065083012, 12.00000000000000000 ) ) ;
#893 = FACE_BOUND ( 'NONE', #18993, .T. ) ;
#894 = DIRECTION ( 'NONE',  ( 0.000000000000000000, -0.000000000000000000, -1.000000000000000000 ) ) ;
#895 = EDGE_LOOP ( 'NONE', ( #14862, #3669, #14526, #19387 ) ) ;
#896 = AXIS2_PLACEMENT_3D ( 'NONE', #20030, #2782, #14749 ) ;
#897 = VERTEX_POINT ( 'NONE', #13506 ) ;
#898 = DIRECTION ( 'NONE',  ( 0.000000000000000000, -0.000000000000000000, 1.000000000000000000 ) ) ;
#899 = PRESENTATION_STYLE_ASSIGNMENT (( #16222 ) ) ;
#900 = DIRECTION ( 'NONE',  ( 0.000000000000000000, 0.000000000000000000, 1.000000000000000000 ) ) ;
#901 = ORIENTED_EDGE ( 'NONE', *, *, #20856, .F. ) ;
#902 = ADVANCED_FACE ( 'NONE', ( #18655 ), #6451, .T. ) ;
#903 = VECTOR ( 'NONE', #12659, 1000.000000000000000 ) ;
#904 = CIRCLE ( 'NONE', #17692, 0.2999999999999999334 ) ;
#905 = AXIS2_PLACEMENT_3D ( 'NONE', #10154, #22028, #6706 ) ;
#906 = ORIENTED_EDGE ( 'NONE', *, *, #11805, .F. ) ;
#907 = EDGE_CURVE ( 'NONE', #10547, #16620, #13283, .T. ) ;
#908 = CARTESIAN_POINT ( 'NONE',  ( 1.824728116533979261, 42.36054587065083155, 51.80876104995653719 ) ) ;
#909 = TOROIDAL_SURFACE ( 'NONE', #13427, 0.05000000000000000278, 0.05000000000000000278 ) ;
#910 = CIRCLE ( 'NONE', #5944, 0.2500000000000004996 ) ;
#911 = CARTESIAN_POINT ( 'NONE',  ( -3.985331397971318079, 42.46645089659917716, 70.50000000000000000 ) ) ;
#912 = CIRCLE ( 'NONE', #14849, 0.2500000000000002220 ) ;
#913 = EDGE_LOOP ( 'NONE', ( #10029, #20388, #14591, #2616 ) ) ;
#914 = DIRECTION ( 'NONE',  ( 0.000000000000000000, 0.000000000000000000, 1.000000000000000000 ) ) ;
#915 = DIRECTION ( 'NONE',  ( -0.000000000000000000, -0.000000000000000000, -1.000000000000000000 ) ) ;
#916 = CARTESIAN_POINT ( 'NONE',  ( -32.20000000000001705, 71.00000000000001421, 3.200000000000000178 ) ) ;
#917 = DIRECTION ( 'NONE',  ( 1.000000000000000000, 0.000000000000000000, 0.000000000000000000 ) ) ;
#918 = LINE ( 'NONE', #2387, #535 ) ;
#919 = AXIS2_PLACEMENT_3D ( 'NONE', #9639, #7857, #7963 ) ;
#920 = VECTOR ( 'NONE', #17928, 1000.000000000000000 ) ;
#921 = EDGE_CURVE ( 'NONE', #19966, #11274, #2492, .T. ) ;
#922 = ORIENTED_EDGE ( 'NONE', *, *, #21017, .F. ) ;
#923 = LINE ( 'NONE', #1045, #4726 ) ;
#924 = LINE ( 'NONE', #19848, #3788 ) ;
#925 = EDGE_CURVE ( 'NONE', #14127, #8942, #8229, .T. ) ;
#926 = ORIENTED_EDGE ( 'NONE', *, *, #4496, .T. ) ;
#927 = ORIENTED_EDGE ( 'NONE', *, *, #17536, .T. ) ;
#928 = ORIENTED_EDGE ( 'NONE', *, *, #2538, .T. ) ;
#929 = DIRECTION ( 'NONE',  ( 1.000000000000000000, 0.000000000000000000, 0.000000000000000000 ) ) ;
#930 = CARTESIAN_POINT ( 'NONE',  ( -17.93704824106378837, -50.11873716947361856, 13.87500000000000000 ) ) ;
#931 = EDGE_LOOP ( 'NONE', ( #3456, #2330, #20937, #8526 ) ) ;
#932 = TOROIDAL_SURFACE ( 'NONE', #14503, 2.274596669241483848, 0.2999999999999999889 ) ;
#933 = AXIS2_PLACEMENT_3D ( 'NONE', #13488, #20112, #16949 ) ;
#934 = CARTESIAN_POINT ( 'NONE',  ( 1.724728116533979616, 43.31054587065082728, 51.75876104995654003 ) ) ;
#935 = CIRCLE ( 'NONE', #18450, 0.2500000000000013323 ) ;
#936 = EDGE_CURVE ( 'NONE', #5793, #10522, #7883, .T. ) ;
#937 = ORIENTED_EDGE ( 'NONE', *, *, #13020, .T. ) ;
#938 = DIRECTION ( 'NONE',  ( 0.2309407893632007824, -0.9729678061520339316, 0.000000000000000000 ) ) ;
#939 = AXIS2_PLACEMENT_3D ( 'NONE', #1566, #15007, #8402 ) ;
#940 = DIRECTION ( 'NONE',  ( -1.000000000000000000, -0.000000000000000000, -0.000000000000000000 ) ) ;
#941 = CARTESIAN_POINT ( 'NONE',  ( -17.95292532278785913, 50.11873716947361856, 13.49999999999999822 ) ) ;
#942 = LINE ( 'NONE', #11873, #13771 ) ;
#943 = CARTESIAN_POINT ( 'NONE',  ( 6.424398693589429399E-15, 58.69165929845684104, 68.50000000000000000 ) ) ;
#944 = DIRECTION ( 'NONE',  ( 1.000000000000000000, 0.000000000000000000, 0.000000000000000000 ) ) ;
#945 = ORIENTED_EDGE ( 'NONE', *, *, #18650, .T. ) ;
#946 = CARTESIAN_POINT ( 'NONE',  ( 3.627054932750481964, -32.61873716947361856, 68.00000000000000000 ) ) ;
#947 = DIRECTION ( 'NONE',  ( 0.000000000000000000, -1.000000000000000000, 0.000000000000000000 ) ) ;
#948 = DIRECTION ( 'NONE',  ( -1.000000000000000000, 2.832483164223434527E-16, 0.000000000000000000 ) ) ;
#949 = CARTESIAN_POINT ( 'NONE',  ( -23.13310673709249343, 45.37789868843801599, 68.50000000000000000 ) ) ;
#950 = EDGE_LOOP ( 'NONE', ( #13983, #7847, #11178, #17308 ) ) ;
#951 = AXIS2_PLACEMENT_3D ( 'NONE', #6007, #19418, #12673 ) ;
#952 = CONICAL_SURFACE ( 'NONE', #6348, 4.575000000000001066, 0.8028514559173934861 ) ;
#953 = CIRCLE ( 'NONE', #17045, 5.000000000000000888 ) ;
#954 = LINE ( 'NONE', #14608, #1961 ) ;
#955 = DIRECTION ( 'NONE',  ( 1.000000000000000000, 0.000000000000000000, 0.000000000000000000 ) ) ;
#956 = CIRCLE ( 'NONE', #18465, 2.767785046117004377 ) ;
#957 = ORIENTED_EDGE ( 'NONE', *, *, #11169, .F. ) ;
#958 = FACE_OUTER_BOUND ( 'NONE', #13559, .T. ) ;
#959 = DIRECTION ( 'NONE',  ( -1.000000000000000000, 0.000000000000000000, 0.000000000000000000 ) ) ;
#960 = EDGE_CURVE ( 'NONE', #17392, #1107, #13582, .T. ) ;
#961 = VERTEX_POINT ( 'NONE', #3224 ) ;
#962 = AXIS2_PLACEMENT_3D ( 'NONE', #14389, #1800, #15446 ) ;
#963 = ORIENTED_EDGE ( 'NONE', *, *, #19556, .F. ) ;
#964 = CARTESIAN_POINT ( 'NONE',  ( 15.95292532278785913, -52.10286008774954780, 13.87499999999999822 ) ) ;
#965 = DIRECTION ( 'NONE',  ( -0.000000000000000000, -0.000000000000000000, 1.000000000000000000 ) ) ;
#966 = ORIENTED_EDGE ( 'NONE', *, *, #11140, .T. ) ;
#967 = AXIS2_PLACEMENT_3D ( 'NONE', #5179, #11980, #18822 ) ;
#968 = ORIENTED_EDGE ( 'NONE', *, *, #6974, .F. ) ;
#969 = DIRECTION ( 'NONE',  ( -0.000000000000000000, -0.000000000000000000, -1.000000000000000000 ) ) ;
#970 = VECTOR ( 'NONE', #17319, 1000.000000000000000 ) ;
#971 = CARTESIAN_POINT ( 'NONE',  ( -23.02398829872514341, -2.157133865694323305, 13.26854876702554442 ) ) ;
#972 = CIRCLE ( 'NONE', #11692, 0.04999999999999991257 ) ;
#973 = EDGE_CURVE ( 'NONE', #13238, #14227, #9667, .T. ) ;
#974 = DIRECTION ( 'NONE',  ( 0.000000000000000000, 0.000000000000000000, 1.000000000000000000 ) ) ;
#975 = AXIS2_PLACEMENT_3D ( 'NONE', #21550, #21655, #6109 ) ;
#976 = CARTESIAN_POINT ( 'NONE',  ( 18.22752199202934520, -38.74634676501045760, 13.79999999999999893 ) ) ;
#977 = AXIS2_PLACEMENT_3D ( 'NONE', #2763, #16516, #13034 ) ;
#978 = DIRECTION ( 'NONE',  ( 1.000000000000000000, 0.000000000000000000, 0.000000000000000000 ) ) ;
#979 = CARTESIAN_POINT ( 'NONE',  ( 14.96174975910707161, 51.61873716947361856, 68.25000000000000000 ) ) ;
#980 = CARTESIAN_POINT ( 'NONE',  ( 28.87540678000427619, 0.000000000000000000, 13.50000000000000000 ) ) ;
#981 = EDGE_LOOP ( 'NONE', ( #16298, #6891, #10402, #11826 ) ) ;
#982 = FACE_OUTER_BOUND ( 'NONE', #19148, .T. ) ;
#983 = EDGE_CURVE ( 'NONE', #1254, #16141, #10054, .T. ) ;
#984 = DIRECTION ( 'NONE',  ( -0.000000000000000000, 0.000000000000000000, 1.000000000000000000 ) ) ;
#985 = LINE ( 'NONE', #21375, #8673 ) ;
#986 = TOROIDAL_SURFACE ( 'NONE', #13498, 0.2500000000000000000, 0.2500000000000000000 ) ;
#987 = VECTOR ( 'NONE', #3190, 1000.000000000000000 ) ;
#988 = AXIS2_PLACEMENT_3D ( 'NONE', #16517, #4339, #20012 ) ;
#989 = LINE ( 'NONE', #8052, #6411 ) ;
#990 = CYLINDRICAL_SURFACE ( 'NONE', #9205, 0.1000000000000028644 ) ;
#991 = ORIENTED_EDGE ( 'NONE', *, *, #21703, .T. ) ;
#992 = CIRCLE ( 'NONE', #13505, 0.2500000000000011657 ) ;
#993 = ORIENTED_EDGE ( 'NONE', *, *, #3228, .F. ) ;
#994 = LINE ( 'NONE', #19926, #21399 ) ;
#995 = AXIS2_PLACEMENT_3D ( 'NONE', #2080, #19097, #10385 ) ;
#996 = EDGE_CURVE ( 'NONE', #16076, #18467, #11, .T. ) ;
#997 = LINE ( 'NONE', #2581, #18287 ) ;
#998 = EDGE_LOOP ( 'NONE', ( #15546, #16742, #6475, #118 ) ) ;
#999 = CARTESIAN_POINT ( 'NONE',  ( -29.13662752439705272, 0.000000000000000000, 0.3000000000000016542 ) ) ;
#1000 = VECTOR ( 'NONE', #16758, 1000.000000000000000 ) ;
#1001 = ORIENTED_EDGE ( 'NONE', *, *, #15403, .T. ) ;
#1002 = DIRECTION ( 'NONE',  ( 0.000000000000000000, 0.000000000000000000, 1.000000000000000000 ) ) ;
#1003 = DIRECTION ( 'NONE',  ( 0.000000000000000000, 0.000000000000000000, 1.000000000000000000 ) ) ;
#1004 = DIRECTION ( 'NONE',  ( 0.000000000000000000, 0.000000000000000000, 1.000000000000000000 ) ) ;
#1005 = CIRCLE ( 'NONE', #16373, 0.3000000000000004885 ) ;
#1006 = AXIS2_PLACEMENT_3D ( 'NONE', #17042, #4976, #21771 ) ;
#1007 = CARTESIAN_POINT ( 'NONE',  ( 23.08502376492392116, 2.484776121502525026, 13.35369709827396001 ) ) ;
#1008 = AXIS2_PLACEMENT_3D ( 'NONE', #17665, #7398, #9176 ) ;
#1009 = DIRECTION ( 'NONE',  ( -0.000000000000000000, -1.000000000000000000, 0.000000000000000000 ) ) ;
#1010 = AXIS2_PLACEMENT_3D ( 'NONE', #11508, #16764, #13725 ) ;
#1011 = EDGE_CURVE ( 'NONE', #15636, #1947, #11074, .T. ) ;
#1012 = FACE_OUTER_BOUND ( 'NONE', #16285, .T. ) ;
#1013 = ADVANCED_FACE ( 'NONE', ( #20460 ), #10015, .T. ) ;
#1014 = FACE_OUTER_BOUND ( 'NONE', #2338, .T. ) ;
#1015 = DIRECTION ( 'NONE',  ( 1.000000000000000000, 0.000000000000000000, 0.000000000000000000 ) ) ;
#1016 = EDGE_CURVE ( 'NONE', #8010, #5585, #5377, .T. ) ;
#1017 = ORIENTED_EDGE ( 'NONE', *, *, #8325, .F. ) ;
#1018 = CARTESIAN_POINT ( 'NONE',  ( -1.824728116533986810, 42.36054587065083155, 27.70876104995653577 ) ) ;
#1019 = VECTOR ( 'NONE', #14846, 1000.000000000000000 ) ;
#1020 = CARTESIAN_POINT ( 'NONE',  ( -25.37540678000426908, 36.74634676501047181, 42.50000000000000000 ) ) ;
#1021 = ORIENTED_EDGE ( 'NONE', *, *, #16712, .T. ) ;
#1022 = ORIENTED_EDGE ( 'NONE', *, *, #853, .F. ) ;
#1023 = CARTESIAN_POINT ( 'NONE',  ( -1.824728116533986810, 42.36054587065083155, 31.70876104995653932 ) ) ;
#1024 = ORIENTED_EDGE ( 'NONE', *, *, #14927, .T. ) ;
#1025 = CIRCLE ( 'NONE', #7842, 0.2999999999999999334 ) ;
#1026 = VERTEX_POINT ( 'NONE', #11494 ) ;
#1027 = EDGE_LOOP ( 'NONE', ( #17597, #18505, #3215, #1779 ) ) ;
#1028 = AXIS2_PLACEMENT_3D ( 'NONE', #17974, #11251, #18205 ) ;
#1029 = ADVANCED_FACE ( 'NONE', ( #14151 ), #17409, .F. ) ;
#1030 = ORIENTED_EDGE ( 'NONE', *, *, #6924, .T. ) ;
#1031 = DIRECTION ( 'NONE',  ( -1.224646799147353207E-16, -0.000000000000000000, -1.000000000000000000 ) ) ;
#1032 = DIRECTION ( 'NONE',  ( 0.000000000000000000, 0.000000000000000000, -1.000000000000000000 ) ) ;
#1033 = VERTEX_POINT ( 'NONE', #8808 ) ;
#1034 = CARTESIAN_POINT ( 'NONE',  ( -1.774728116533986766, 43.31054587065082728, 33.66679706732590915 ) ) ;
#1035 = EDGE_CURVE ( 'NONE', #4495, #11313, #12847, .T. ) ;
#1036 = B_SPLINE_CURVE_WITH_KNOTS ( 'NONE', 3,
 ( #16940, #11680, #11466, #18737 ),
 .UNSPECIFIED., .F., .F.,
 ( 4, 4 ),
 ( 0.001759598105097497350, 0.004588913567995311395 ),
 .UNSPECIFIED. ) ;
#1037 = CARTESIAN_POINT ( 'NONE',  ( 0.000000000000000000, -32.11873716947361856, 109.6002446535588319 ) ) ;
#1038 = CIRCLE ( 'NONE', #19641, 0.2999999999999999334 ) ;
#1039 = EDGE_CURVE ( 'NONE', #20933, #14982, #10815, .T. ) ;
#1040 = CARTESIAN_POINT ( 'NONE',  ( 14.98586301832698808, 51.95135570414442583, 13.85537332152988554 ) ) ;
#1041 = CARTESIAN_POINT ( 'NONE',  ( 34.39999999999998437, -85.00000000000000000, 79.39999999999999147 ) ) ;
#1042 = CARTESIAN_POINT ( 'NONE',  ( -23.02398829872514341, 2.502141052783100061, 13.57900107139873747 ) ) ;
#1043 = EDGE_CURVE ( 'NONE', #14452, #17182, #21467, .T. ) ;
#1044 = ORIENTED_EDGE ( 'NONE', *, *, #10066, .T. ) ;
#1045 = CARTESIAN_POINT ( 'NONE',  ( 14.96174975910707161, 41.81054587065082728, 68.25000000000000000 ) ) ;
#1046 = LINE ( 'NONE', #18163, #21312 ) ;
#1047 = VERTEX_POINT ( 'NONE', #175 ) ;
#1048 = ORIENTED_EDGE ( 'NONE', *, *, #3785, .F. ) ;
#1049 = ORIENTED_EDGE ( 'NONE', *, *, #15440, .T. ) ;
#1050 = LINE ( 'NONE', #14696, #17766 ) ;
#1051 = CYLINDRICAL_SURFACE ( 'NONE', #21049, 0.04999999999999991257 ) ;
#1052 = ORIENTED_EDGE ( 'NONE', *, *, #11319, .T. ) ;
#1053 = TOROIDAL_SURFACE ( 'NONE', #13353, 0.7000000000000000666, 0.2999999999999999889 ) ;
#1054 = CARTESIAN_POINT ( 'NONE',  ( 9.141460742840918030, -33.43424481021354921, 42.50000000000000000 ) ) ;
#1055 = AXIS2_PLACEMENT_3D ( 'NONE', #3798, #2111, #5597 ) ;
#1056 = PRESENTATION_LAYER_ASSIGNMENT (  '', '', ( #10722 ) ) ;
#1057 = AXIS2_PLACEMENT_3D ( 'NONE', #12568, #3986, #19196 ) ;
#1058 = ORIENTED_EDGE ( 'NONE', *, *, #9168, .F. ) ;
#1059 = DIRECTION ( 'NONE',  ( 1.000000000000000000, 0.000000000000000000, 0.000000000000000000 ) ) ;
#1060 = EDGE_CURVE ( 'NONE', #18170, #3171, #20681, .T. ) ;
#1061 = DIRECTION ( 'NONE',  ( 1.000000000000000000, 0.000000000000000000, 0.000000000000000000 ) ) ;
#1062 = DIRECTION ( 'NONE',  ( -1.000000000000000000, -0.000000000000000000, -0.000000000000000000 ) ) ;
#1063 = DIRECTION ( 'NONE',  ( -1.000000000000000000, 0.000000000000000000, 0.000000000000000000 ) ) ;
#1064 = CARTESIAN_POINT ( 'NONE',  ( -1.724728116533986721, 42.36054587065083155, 43.80876104995653719 ) ) ;
#1065 = ORIENTED_EDGE ( 'NONE', *, *, #7876, .T. ) ;
#1066 = DIRECTION ( 'NONE',  ( 1.000000000000000000, 0.000000000000000000, 0.000000000000000000 ) ) ;
#1067 = FACE_OUTER_BOUND ( 'NONE', #16797, .T. ) ;
#1068 = DIRECTION ( 'NONE',  ( 1.000000000000000000, 0.000000000000000000, 0.000000000000000000 ) ) ;
#1069 = CARTESIAN_POINT ( 'NONE',  ( -31.07535336168307083, 84.25171694722490656, 13.75000000000000000 ) ) ;
#1070 = VERTEX_POINT ( 'NONE', #4000 ) ;
#1071 = CYLINDRICAL_SURFACE ( 'NONE', #15191, 0.2999999999999999889 ) ;
#1072 = CARTESIAN_POINT ( 'NONE',  ( -1.724728116533986721, 43.26054587065083012, 53.71679706732590631 ) ) ;
#1073 = EDGE_CURVE ( 'NONE', #4505, #15052, #1868, .T. ) ;
#1074 = AXIS2_PLACEMENT_3D ( 'NONE', #12909, #13136, #19754 ) ;
#1075 = ORIENTED_EDGE ( 'NONE', *, *, #195, .F. ) ;
#1076 = AXIS2_PLACEMENT_3D ( 'NONE', #15904, #2049, #5659 ) ;
#1077 = CARTESIAN_POINT ( 'NONE',  ( 28.87540678000427619, 6.494748934539263274, 13.19999999999999929 ) ) ;
#1078 = CARTESIAN_POINT ( 'NONE',  ( 29.37540678000427619, 5.299999999999999822, 7.200000000000000178 ) ) ;
#1079 = EDGE_LOOP ( 'NONE', ( #1272, #8804, #3579, #12493, #1570 ) ) ;
#1080 = ORIENTED_EDGE ( 'NONE', *, *, #7728, .F. ) ;
#1081 = ORIENTED_EDGE ( 'NONE', *, *, #13056, .F. ) ;
#1082 = CARTESIAN_POINT ( 'NONE',  ( 0.000000000000000000, 68.70000000000001705, 0.000000000000000000 ) ) ;
#1083 = CARTESIAN_POINT ( 'NONE',  ( 34.69999999999998863, 85.00000000000000000, 79.39999999999999147 ) ) ;
#1084 = ORIENTED_EDGE ( 'NONE', *, *, #5957, .T. ) ;
#1085 = ORIENTED_EDGE ( 'NONE', *, *, #1135, .F. ) ;
#1086 = CARTESIAN_POINT ( 'NONE',  ( -8.638906393579159015, 41.42245079618239600, 68.06527860057354928 ) ) ;
#1087 = CIRCLE ( 'NONE', #16451, 0.5999999999999999778 ) ;
#1088 = ADVANCED_FACE ( 'NONE', ( #10487 ), #2301, .T. ) ;
#1089 = CARTESIAN_POINT ( 'NONE',  ( -29.17540678000427690, 6.499884319688664647, 7.500000000000000000 ) ) ;
#1090 = FACE_OUTER_BOUND ( 'NONE', #20472, .T. ) ;
#1091 = AXIS2_PLACEMENT_3D ( 'NONE', #8071, #4606, #6410 ) ;
#1092 = CARTESIAN_POINT ( 'NONE',  ( -4.127054932750482408, -33.43424481021354921, 42.50000000000000000 ) ) ;
#1093 = EDGE_CURVE ( 'NONE', #11281, #17520, #16861, .T. ) ;
#1094 = CARTESIAN_POINT ( 'NONE',  ( 29.69597781366221767, 58.94165929845684104, 68.75000000000000000 ) ) ;
#1095 = DIRECTION ( 'NONE',  ( 0.000000000000000000, 1.000000000000000000, -0.000000000000000000 ) ) ;
#1096 = CARTESIAN_POINT ( 'NONE',  ( -10.20831163238817219, 41.92645089659918511, 70.88527860057354246 ) ) ;
#1097 = DIRECTION ( 'NONE',  ( 0.000000000000000000, 0.000000000000000000, 1.000000000000000000 ) ) ;
#1098 = DIRECTION ( 'NONE',  ( 1.000000000000000000, 0.000000000000000000, -0.000000000000000000 ) ) ;
#1099 = ORIENTED_EDGE ( 'NONE', *, *, #425, .F. ) ;
#1100 = DIRECTION ( 'NONE',  ( -0.000000000000000000, 0.000000000000000000, 1.000000000000000000 ) ) ;
#1101 = DIRECTION ( 'NONE',  ( 0.000000000000000000, -1.000000000000000000, 0.000000000000000000 ) ) ;
#1102 = CYLINDRICAL_SURFACE ( 'NONE', #5106, 1.999999999999991340 ) ;
#1103 = ORIENTED_EDGE ( 'NONE', *, *, #1983, .T. ) ;
#1104 = FACE_OUTER_BOUND ( 'NONE', #6482, .T. ) ;
#1105 = LINE ( 'NONE', #14981, #13124 ) ;
#1106 = VECTOR ( 'NONE', #1009, 1000.000000000000000 ) ;
#1107 = VERTEX_POINT ( 'NONE', #17194 ) ;
#1108 = EDGE_CURVE ( 'NONE', #18032, #16813, #15430, .T. ) ;
#1109 = ORIENTED_EDGE ( 'NONE', *, *, #20925, .T. ) ;
#1110 = LINE ( 'NONE', #19462, #5275 ) ;
#1111 = ADVANCED_FACE ( 'NONE', ( #12353 ), #17922, .T. ) ;
#1112 = AXIS2_PLACEMENT_3D ( 'NONE', #16943, #12011, #18859 ) ;
#1113 = DIRECTION ( 'NONE',  ( 2.343267634472166901E-16, 0.8949343913984426635, 0.4461977533474357771 ) ) ;
#1114 = CARTESIAN_POINT ( 'NONE',  ( 1.774728116533979438, 43.31054587065082728, 47.80876104995653719 ) ) ;
#1115 = AXIS2_PLACEMENT_3D ( 'NONE', #14128, #5670, #14252 ) ;
#1116 = DIRECTION ( 'NONE',  ( -0.000000000000000000, -0.000000000000000000, 1.000000000000000000 ) ) ;
#1117 = CARTESIAN_POINT ( 'NONE',  ( -29.17540678000427690, 0.000000000000000000, 7.799999999999999822 ) ) ;
#1118 = CARTESIAN_POINT ( 'NONE',  ( -9.718906393579157310, 41.58710221366784054, 69.00503344894293889 ) ) ;
#1119 = DIRECTION ( 'NONE',  ( 0.000000000000000000, 0.000000000000000000, 1.000000000000000000 ) ) ;
#1120 = DIRECTION ( 'NONE',  ( -1.000000000000000000, -0.000000000000000000, -0.000000000000000000 ) ) ;
#1121 = CARTESIAN_POINT ( 'NONE',  ( 17.45292532278785913, 34.11873716947361856, 68.50000000000000000 ) ) ;
#1122 = DIRECTION ( 'NONE',  ( -0.000000000000000000, -1.000000000000000000, -0.000000000000000000 ) ) ;
#1123 = CIRCLE ( 'NONE', #20445, 0.1000000000000028644 ) ;
#1124 = EDGE_CURVE ( 'NONE', #19800, #11695, #15727, .T. ) ;
#1125 = AXIS2_PLACEMENT_3D ( 'NONE', #4401, #4634, #6207 ) ;
#1126 = ORIENTED_EDGE ( 'NONE', *, *, #14675, .T. ) ;
#1127 = DIRECTION ( 'NONE',  ( 1.000000000000000000, 0.000000000000000000, -1.224646799147353207E-16 ) ) ;
#1128 = AXIS2_PLACEMENT_3D ( 'NONE', #16483, #1149, #7994 ) ;
#1129 = CARTESIAN_POINT ( 'NONE',  ( 1.724728116533979838, 42.36054587065083155, 41.71679706732590631 ) ) ;
#1130 = ORIENTED_EDGE ( 'NONE', *, *, #2625, .F. ) ;
#1131 = EDGE_LOOP ( 'NONE', ( #5506, #6483, #9261, #21023, #17043, #11707, #1139, #7153 ) ) ;
#1132 = DIRECTION ( 'NONE',  ( -1.000000000000000000, 0.000000000000000000, 0.000000000000000000 ) ) ;
#1133 = ORIENTED_EDGE ( 'NONE', *, *, #9281, .F. ) ;
#1134 = ORIENTED_EDGE ( 'NONE', *, *, #14013, .F. ) ;
#1135 = EDGE_CURVE ( 'NONE', #7001, #7855, #19018, .T. ) ;
#1136 = EDGE_CURVE ( 'NONE', #20345, #10550, #18886, .T. ) ;
#1137 = EDGE_LOOP ( 'NONE', ( #8614, #20350, #9374, #13119, #17297, #5583, #19057, #13369, #18610, #9638, #5260, #1739, #4437, #4162, #14733, #9061, #11584, #10946, #4991, #16370, #21549, #21887, #415, #16787 ) ) ;
#1138 = EDGE_CURVE ( 'NONE', #8252, #11281, #11139, .T. ) ;
#1139 = ORIENTED_EDGE ( 'NONE', *, *, #12018, .T. ) ;
#1140 = CARTESIAN_POINT ( 'NONE',  ( -14.66895125224955976, -51.92349729544097414, 13.50000000000000000 ) ) ;
#1141 = VECTOR ( 'NONE', #6596, 1000.000000000000000 ) ;
#1142 = DIRECTION ( 'NONE',  ( 0.000000000000000000, 0.000000000000000000, 1.000000000000000000 ) ) ;
#1143 = ORIENTED_EDGE ( 'NONE', *, *, #20400, .T. ) ;
#1144 = CARTESIAN_POINT ( 'NONE',  ( 32.50000000000002132, 72.00000000000001421, 1.800000000000000044 ) ) ;
#1145 = DIRECTION ( 'NONE',  ( 0.000000000000000000, 0.000000000000000000, 1.000000000000000000 ) ) ;
#1146 = DIRECTION ( 'NONE',  ( 0.000000000000000000, -1.000000000000000000, 0.000000000000000000 ) ) ;
#1147 = EDGE_CURVE ( 'NONE', #2755, #12023, #21164, .T. ) ;
#1148 = VERTEX_POINT ( 'NONE', #12247 ) ;
#1149 = DIRECTION ( 'NONE',  ( -1.000000000000000000, -0.000000000000000000, -0.000000000000000000 ) ) ;
#1150 = VERTEX_POINT ( 'NONE', #15830 ) ;
#1151 = ORIENTED_EDGE ( 'NONE', *, *, #13368, .T. ) ;
#1152 = VERTEX_POINT ( 'NONE', #19098 ) ;
#1153 = DIRECTION ( 'NONE',  ( -0.000000000000000000, -0.000000000000000000, -1.000000000000000000 ) ) ;
#1154 = CARTESIAN_POINT ( 'NONE',  ( 27.37540678000427619, 10.94079601157914539, 13.79999999999999893 ) ) ;
#1155 = ORIENTED_EDGE ( 'NONE', *, *, #11973, .T. ) ;
#1156 = DIRECTION ( 'NONE',  ( 1.000000000000000000, 0.000000000000000000, 0.000000000000000000 ) ) ;
#1157 = ADVANCED_FACE ( 'NONE', ( #20892 ), #3766, .T. ) ;
#1158 = EDGE_CURVE ( 'NONE', #22102, #16814, #5693, .T. ) ;
#1159 = ORIENTED_EDGE ( 'NONE', *, *, #20469, .T. ) ;
#1160 = CARTESIAN_POINT ( 'NONE',  ( -30.79999999999999361, -85.00000000000000000, 0.3000000000000002665 ) ) ;
#1161 = CARTESIAN_POINT ( 'NONE',  ( -1.724728116533986721, 43.31054587065082728, 49.71679706732589921 ) ) ;
#1162 = EDGE_CURVE ( 'NONE', #18311, #2722, #418, .T. ) ;
#1163 = CARTESIAN_POINT ( 'NONE',  ( -15.21174975910705207, 51.86873716947361856, 14.00000000000000000 ) ) ;
#1164 = DIRECTION ( 'NONE',  ( 0.000000000000000000, -0.000000000000000000, -1.000000000000000000 ) ) ;
#1165 = VERTEX_POINT ( 'NONE', #14599 ) ;
#1166 = DIRECTION ( 'NONE',  ( 0.000000000000000000, 0.000000000000000000, -1.000000000000000000 ) ) ;
#1167 = DIRECTION ( 'NONE',  ( 0.000000000000000000, -1.000000000000000000, 0.000000000000000000 ) ) ;
#1168 = CARTESIAN_POINT ( 'NONE',  ( -15.05282292896043295, 52.05812657117055409, 13.87232935072191786 ) ) ;
#1169 = FACE_OUTER_BOUND ( 'NONE', #18177, .T. ) ;
#1170 = VERTEX_POINT ( 'NONE', #17956 ) ;
#1171 = DIRECTION ( 'NONE',  ( 1.000000000000000000, 0.000000000000000000, 0.000000000000000000 ) ) ;
#1172 = DIRECTION ( 'NONE',  ( 0.000000000000000000, 0.000000000000000000, -1.000000000000000000 ) ) ;
#1173 = EDGE_CURVE ( 'NONE', #9535, #10367, #771, .T. ) ;
#1174 = ORIENTED_EDGE ( 'NONE', *, *, #15120, .T. ) ;
#1175 = FACE_OUTER_BOUND ( 'NONE', #21833, .T. ) ;
#1176 = CYLINDRICAL_SURFACE ( 'NONE', #16290, 0.05000000000000143219 ) ;
#1177 = VERTEX_POINT ( 'NONE', #2629 ) ;
#1178 = VERTEX_POINT ( 'NONE', #7909 ) ;
#1179 = ORIENTED_EDGE ( 'NONE', *, *, #2808, .T. ) ;
#1180 = CARTESIAN_POINT ( 'NONE',  ( -15.12826760881917387, 51.99271056040087302, 13.49999999999999822 ) ) ;
#1181 = FACE_OUTER_BOUND ( 'NONE', #5161, .T. ) ;
#1182 = EDGE_CURVE ( 'NONE', #22, #14293, #16123, .T. ) ;
#1183 = LINE ( 'NONE', #12697, #18158 ) ;
#1184 = ORIENTED_EDGE ( 'NONE', *, *, #9168, .T. ) ;
#1185 = EDGE_LOOP ( 'NONE', ( #14887, #223, #21649, #15891, #11578, #7138, #9352, #4309, #18651, #11198, #21910, #11567, #14634, #6720, #9249, #18703, #5681, #4978, #21522, #20267, #20160, #10856, #11371, #7817 ) ) ;
#1186 = CARTESIAN_POINT ( 'NONE',  ( 1.824728116533979261, 42.36054587065083155, 31.80876104995653719 ) ) ;
#1187 = ADVANCED_FACE ( 'NONE', ( #2416 ), #21122, .F. ) ;
#1188 = DIRECTION ( 'NONE',  ( 0.000000000000000000, 0.000000000000000000, -1.000000000000000000 ) ) ;
#1189 = DIRECTION ( 'NONE',  ( 0.000000000000000000, -1.000000000000000000, 0.000000000000000000 ) ) ;
#1190 = DIRECTION ( 'NONE',  ( -1.000000000000000000, 0.000000000000000000, -8.673617379884034239E-17 ) ) ;
#1191 = CARTESIAN_POINT ( 'NONE',  ( 0.000000000000000000, 42.31054587065082728, 43.75876104995654003 ) ) ;
#1192 = CYLINDRICAL_SURFACE ( 'NONE', #6547, 0.05000000000000143219 ) ;
#1193 = FACE_OUTER_BOUND ( 'NONE', #7814, .T. ) ;
#1194 = CARTESIAN_POINT ( 'NONE',  ( -15.95292532278785913, -50.11873716947361856, 13.79999999999999893 ) ) ;
#1195 = VERTEX_POINT ( 'NONE', #17846 ) ;
#1196 = DIRECTION ( 'NONE',  ( -1.000000000000000000, -0.000000000000000000, -0.000000000000000000 ) ) ;
#1197 = DIRECTION ( 'NONE',  ( 1.000000000000000000, -0.000000000000000000, 0.000000000000000000 ) ) ;
#1198 = ORIENTED_EDGE ( 'NONE', *, *, #110, .F. ) ;
#1199 = CARTESIAN_POINT ( 'NONE',  ( 23.04273156199908357, 2.261510999192738680, 13.50000000000000000 ) ) ;
#1200 = EDGE_CURVE ( 'NONE', #4392, #18664, #16048, .T. ) ;
#1202 = AXIS2_PLACEMENT_3D ( 'NONE', #20688, #17852, #5899 ) ;
#1201 = DIRECTION ( 'NONE',  ( 0.000000000000000000, -0.000000000000000000, 1.000000000000000000 ) ) ;
#1203 = ORIENTED_EDGE ( 'NONE', *, *, #17279, .F. ) ;
#1204 = EDGE_CURVE ( 'NONE', #19855, #10005, #21882, .T. ) ;
#1205 = EDGE_CURVE ( 'NONE', #6175, #20684, #13282, .T. ) ;
#1206 = ORIENTED_EDGE ( 'NONE', *, *, #16364, .T. ) ;
#1207 = DIRECTION ( 'NONE',  ( -1.000000000000000000, 0.000000000000000000, 0.000000000000000000 ) ) ;
#1208 = ORIENTED_EDGE ( 'NONE', *, *, #22003, .F. ) ;
#1209 = AXIS2_PLACEMENT_3D ( 'NONE', #10527, #3372, #20832 ) ;
#1210 = CIRCLE ( 'NONE', #4088, 0.1000000000000028644 ) ;
#1211 = CARTESIAN_POINT ( 'NONE',  ( 3.127054932750481964, -32.61873716947361856, 68.00000000000000000 ) ) ;
#1212 = ORIENTED_EDGE ( 'NONE', *, *, #1930, .T. ) ;
#1213 = CARTESIAN_POINT ( 'NONE',  ( -9.178906393579158163, 42.46645089659918426, 68.06527860057354928 ) ) ;
#1214 = DIRECTION ( 'NONE',  ( 0.000000000000000000, 0.000000000000000000, 1.000000000000000000 ) ) ;
#1215 = CARTESIAN_POINT ( 'NONE',  ( 23.18291235612340628, 2.947575143997193337, 13.45754841673216973 ) ) ;
#1216 = EDGE_CURVE ( 'NONE', #12212, #1750, #21225, .T. ) ;
#1217 = CYLINDRICAL_SURFACE ( 'NONE', #4984, 0.2999999999999999334 ) ;
#1218 = DIRECTION ( 'NONE',  ( 0.000000000000000000, 1.000000000000000000, 0.000000000000000000 ) ) ;
#1219 = FACE_OUTER_BOUND ( 'NONE', #9911, .T. ) ;
#1220 = DIRECTION ( 'NONE',  ( 1.000000000000000000, 0.000000000000000000, 0.000000000000000000 ) ) ;
#1221 = DIRECTION ( 'NONE',  ( -0.2309407893632008379, 0.9729678061520339316, 0.000000000000000000 ) ) ;
#1222 = AXIS2_PLACEMENT_3D ( 'NONE', #14000, #17477, #12302 ) ;
#1223 = EDGE_CURVE ( 'NONE', #21686, #13159, #1495, .T. ) ;
#1224 = ORIENTED_EDGE ( 'NONE', *, *, #17536, .F. ) ;
#1225 = CARTESIAN_POINT ( 'NONE',  ( 14.96174975910707161, 41.81054587065082728, 68.25000000000000000 ) ) ;
#1226 = ORIENTED_EDGE ( 'NONE', *, *, #2404, .F. ) ;
#1227 = DIRECTION ( 'NONE',  ( 0.000000000000000000, 0.000000000000000000, -1.000000000000000000 ) ) ;
#1228 = PRODUCT ( 'Lampshade', 'Lampshade', '', ( #20396 ) ) ;
#1229 = EDGE_CURVE ( 'NONE', #10573, #1591, #8640, .T. ) ;
#1230 = CYLINDRICAL_SURFACE ( 'NONE', #15654, 1.000000000000000888 ) ;
#1231 = ORIENTED_EDGE ( 'NONE', *, *, #21219, .T. ) ;
#1232 = EDGE_LOOP ( 'NONE', ( #17781, #13374, #17762, #19889 ) ) ;
#1233 = DIRECTION ( 'NONE',  ( 0.000000000000000000, 0.000000000000000000, -1.000000000000000000 ) ) ;
#1234 =( NAMED_UNIT ( * ) SI_UNIT ( $, .STERADIAN. ) SOLID_ANGLE_UNIT ( ) );
#1235 = UNCERTAINTY_MEASURE_WITH_UNIT (LENGTH_MEASURE( 1.000000000000000082E-05 ), #13754, 'distance_accuracy_value', 'NONE');
#1236 = ORIENTED_EDGE ( 'NONE', *, *, #17216, .T. ) ;
#1237 = DIRECTION ( 'NONE',  ( 0.000000000000000000, 0.000000000000000000, 1.000000000000000000 ) ) ;
#1238 = ORIENTED_EDGE ( 'NONE', *, *, #5842, .T. ) ;
#1239 = VERTEX_POINT ( 'NONE', #21334 ) ;
#1240 = ORIENTED_EDGE ( 'NONE', *, *, #195, .T. ) ;
#1241 = CARTESIAN_POINT ( 'NONE',  ( 15.00289696508457915, -51.98500081155935248, 13.86091301037357226 ) ) ;
#1242 = EDGE_CURVE ( 'NONE', #19336, #5684, #1123, .T. ) ;
#1243 = CARTESIAN_POINT ( 'NONE',  ( 9.641460742840918030, 32.61873716947361856, 68.00000000000000000 ) ) ;
#1244 = ORIENTED_EDGE ( 'NONE', *, *, #4424, .F. ) ;
#1245 = DIRECTION ( 'NONE',  ( 1.000000000000000000, 0.000000000000000000, 0.000000000000000000 ) ) ;
#1246 = CARTESIAN_POINT ( 'NONE',  ( 14.96174975910707161, 51.86873716947361856, 68.00000000000000000 ) ) ;
#1247 = CARTESIAN_POINT ( 'NONE',  ( 1.774728116533979660, 43.31054587065082728, 41.66679706732590915 ) ) ;
#1248 = CARTESIAN_POINT ( 'NONE',  ( -29.01849620351543280, 6.499161877189502334, 7.532606289305298297 ) ) ;
#1249 = CIRCLE ( 'NONE', #13755, 0.1000000000000028644 ) ;
#1250 = ADVANCED_FACE ( 'NONE', ( #9350 ), #4209, .F. ) ;
#1251 = LINE ( 'NONE', #3054, #14348 ) ;
#1252 = VERTEX_POINT ( 'NONE', #831 ) ;
#1253 = VECTOR ( 'NONE', #14129, 1000.000000000000000 ) ;
#1254 = VERTEX_POINT ( 'NONE', #16258 ) ;
#1255 = CIRCLE ( 'NONE', #15897, 4.575000000000001066 ) ;
#1256 = AXIS2_PLACEMENT_3D ( 'NONE', #14931, #16393, #4420 ) ;
#1257 = ORIENTED_EDGE ( 'NONE', *, *, #16855, .T. ) ;
#1258 = DIRECTION ( 'NONE',  ( 0.000000000000000000, 0.000000000000000000, 1.000000000000000000 ) ) ;
#1259 = FACE_OUTER_BOUND ( 'NONE', #20406, .T. ) ;
#1260 = EDGE_LOOP ( 'NONE', ( #12691, #3895, #19367, #16632 ) ) ;
#1261 = DIRECTION ( 'NONE',  ( -0.000000000000000000, -1.000000000000000000, -0.000000000000000000 ) ) ;
#1262 = EDGE_LOOP ( 'NONE', ( #12377, #121, #4226, #1320 ) ) ;
#1263 = DIRECTION ( 'NONE',  ( 0.000000000000000000, 0.000000000000000000, 1.000000000000000000 ) ) ;
#1264 = VECTOR ( 'NONE', #3007, 1000.000000000000000 ) ;
#1265 = AXIS2_PLACEMENT_3D ( 'NONE', #6227, #13011, #18707 ) ;
#1266 = LINE ( 'NONE', #11350, #12361 ) ;
#1267 = EDGE_CURVE ( 'NONE', #14159, #9535, #14472, .T. ) ;
#1268 = DIRECTION ( 'NONE',  ( 0.000000000000000000, 0.000000000000000000, 1.000000000000000000 ) ) ;
#1269 = CIRCLE ( 'NONE', #3432, 2.500000000000002220 ) ;
#1270 = DIRECTION ( 'NONE',  ( 0.000000000000000000, 1.000000000000000000, 0.000000000000000000 ) ) ;
#1271 = AXIS2_PLACEMENT_3D ( 'NONE', #2495, #2949, #11100 ) ;
#1272 = ORIENTED_EDGE ( 'NONE', *, *, #5763, .F. ) ;
#1273 = DIRECTION ( 'NONE',  ( -1.000000000000000000, 0.000000000000000000, 0.000000000000000000 ) ) ;
#1274 = CARTESIAN_POINT ( 'NONE',  ( 9.641460742840918030, -32.61873716947361856, 68.50000000000000000 ) ) ;
#1275 = FACE_OUTER_BOUND ( 'NONE', #544, .T. ) ;
#1276 = DIRECTION ( 'NONE',  ( 1.000000000000000000, 0.000000000000000000, 0.000000000000000000 ) ) ;
#1277 = ORIENTED_EDGE ( 'NONE', *, *, #17002, .T. ) ;
#1278 = CARTESIAN_POINT ( 'NONE',  ( -29.13662752439705272, 4.700000000000000178, 3.799999999999999822 ) ) ;
#1279 = CARTESIAN_POINT ( 'NONE',  ( -29.50000000000002132, 2.473451120191013430, -150.0833101980363722 ) ) ;
#1280 = ADVANCED_FACE ( 'NONE', ( #21453 ), #6124, .T. ) ;
#1281 = EDGE_CURVE ( 'NONE', #16343, #19005, #21564, .T. ) ;
#1282 = ORIENTED_EDGE ( 'NONE', *, *, #19556, .T. ) ;
#1283 = CARTESIAN_POINT ( 'NONE',  ( -30.67540678000428045, -6.000000000000000000, 3.500000000000000000 ) ) ;
#1284 = EDGE_CURVE ( 'NONE', #17663, #13966, #8905, .T. ) ;
#1285 = DIRECTION ( 'NONE',  ( 1.224646799147353207E-16, 0.000000000000000000, 1.000000000000000000 ) ) ;
#1286 = ORIENTED_EDGE ( 'NONE', *, *, #4525, .F. ) ;
#1287 = AXIS2_PLACEMENT_3D ( 'NONE', #13763, #5302, #10764 ) ;
#1288 = ORIENTED_EDGE ( 'NONE', *, *, #6245, .F. ) ;
#1289 = AXIS2_PLACEMENT_3D ( 'NONE', #14870, #21727, #16657 ) ;
#1290 = ORIENTED_EDGE ( 'NONE', *, *, #17720, .F. ) ;
#1291 = DIRECTION ( 'NONE',  ( 0.000000000000000000, 1.000000000000000000, 0.000000000000000000 ) ) ;
#1292 = EDGE_CURVE ( 'NONE', #20277, #1170, #19360, .T. ) ;
#1293 = LINE ( 'NONE', #18411, #5741 ) ;
#1294 = ORIENTED_EDGE ( 'NONE', *, *, #9177, .F. ) ;
#1295 = VECTOR ( 'NONE', #11323, 1000.000000000000000 ) ;
#1296 = ORIENTED_EDGE ( 'NONE', *, *, #11231, .T. ) ;
#1297 = DIRECTION ( 'NONE',  ( 1.000000000000000000, 0.000000000000000000, 0.000000000000000000 ) ) ;
#1298 = EDGE_CURVE ( 'NONE', #11071, #583, #7567, .T. ) ;
#1299 = CARTESIAN_POINT ( 'NONE',  ( 9.641460742840918030, 32.11873716947361856, 109.6002446535588319 ) ) ;
#1300 = CARTESIAN_POINT ( 'NONE',  ( -23.02398829872513986, -2.877181859310994128, 13.71509684061244450 ) ) ;
#1301 = CARTESIAN_POINT ( 'NONE',  ( -17.45292532278785913, 0.000000000000000000, 68.00000000000000000 ) ) ;
#1302 = CIRCLE ( 'NONE', #16664, 1.500000000000001332 ) ;
#1303 = CIRCLE ( 'NONE', #13804, 0.2500000000000002220 ) ;
#1304 = AXIS2_PLACEMENT_3D ( 'NONE', #3872, #10571, #7334 ) ;
#1305 = DIRECTION ( 'NONE',  ( 0.000000000000000000, 0.000000000000000000, -1.000000000000000000 ) ) ;
#1306 = VECTOR ( 'NONE', #14026, 1000.000000000000000 ) ;
#1307 = FACE_OUTER_BOUND ( 'NONE', #11690, .T. ) ;
#1308 = CARTESIAN_POINT ( 'NONE',  ( -1.724728116533986721, 43.31054587065082728, 35.75876104995654003 ) ) ;
#1309 = DIRECTION ( 'NONE',  ( -1.000000000000000000, 0.000000000000000000, 0.000000000000000000 ) ) ;
#1310 = CARTESIAN_POINT ( 'NONE',  ( -1.724728116533986721, 43.31054587065082728, 47.75876104995653293 ) ) ;
#1311 = EDGE_LOOP ( 'NONE', ( #16611, #19884, #4952, #13956 ) ) ;
#1312 = FACE_OUTER_BOUND ( 'NONE', #16989, .T. ) ;
#1313 = ADVANCED_FACE ( 'NONE', ( #22086 ), #3381, .T. ) ;
#1314 = CARTESIAN_POINT ( 'NONE',  ( -1.824728116533986810, 43.31054587065082728, 31.80876104995653719 ) ) ;
#1315 = DIRECTION ( 'NONE',  ( -5.192538640813645496E-17, 1.000000000000000000, 6.359025825921378559E-33 ) ) ;
#1316 = EDGE_LOOP ( 'NONE', ( #8205, #5330, #1841, #11143 ) ) ;
#1318 = ADVANCED_FACE ( 'NONE', ( #15754 ), #20072, .T. ) ;
#1317 = CARTESIAN_POINT ( 'NONE',  ( -27.67540678000428045, 7.839012376739720627E-15, 13.79999999999999893 ) ) ;
#1319 = CARTESIAN_POINT ( 'NONE',  ( 28.87540678000427619, -6.494748934539263274, 13.19999999999999929 ) ) ;
#1320 = ORIENTED_EDGE ( 'NONE', *, *, #4061, .T. ) ;
#1321 = CLOSED_SHELL ( 'NONE', ( #18011, #21293, #21672, #5432, #6026, #18113, #10541, #12822, #6337, #10935, #18987, #12640, #20548, #19431, #3631, #21052, #18522, #8958, #13304, #3118, #4749, #6859, #4343, #11185, #5214, #5607, #21919, #16779, #6308, #15466, #14203, #452, #5743, #8639, #8664, #10211, #10888, #14993, #4284, #14406, #19041, #19233, #10753, #8394, #13839, #1993, #12774, #10492, #12729, #5683, #17441, #8705, #17229, #21751, #17087, #2750, #8864, #8180, #13650, #9553, #19453, #4425, #17157, #4152, #7292, #1013, #13633, #2457, #20762, #2460, #16647, #1862, #3376 ) ) ;
#1322 = AXIS2_PLACEMENT_3D ( 'NONE', #21500, #17998, #7849 ) ;
#1323 = AXIS2_PLACEMENT_3D ( 'NONE', #2062, #14130, #8903 ) ;
#1324 = ORIENTED_EDGE ( 'NONE', *, *, #3556, .F. ) ;
#1325 = CARTESIAN_POINT ( 'NONE',  ( 29.20000000000002061, -2.799282752659324025, 0.000000000000000000 ) ) ;
#1326 = AXIS2_PLACEMENT_3D ( 'NONE', #15402, #6923, #5230 ) ;
#1327 = VERTEX_POINT ( 'NONE', #17558 ) ;
#1328 = CIRCLE ( 'NONE', #4199, 0.2499999999999961975 ) ;
#1329 = CARTESIAN_POINT ( 'NONE',  ( -9.718906393579157310, 43.49585613540820361, 70.88527860057354246 ) ) ;
#1330 = CARTESIAN_POINT ( 'NONE',  ( 29.13662752439705272, 5.000000000000000000, 7.500000000000000000 ) ) ;
#1331 = PLANE ( 'NONE',  #11714 ) ;
#1332 = EDGE_CURVE ( 'NONE', #6460, #18368, #11121, .T. ) ;
#1333 = FACE_OUTER_BOUND ( 'NONE', #9515, .T. ) ;
#1334 = AXIS2_PLACEMENT_3D ( 'NONE', #8386, #10299, #20043 ) ;
#1335 = AXIS2_PLACEMENT_3D ( 'NONE', #21037, #19346, #15749 ) ;
#1336 = CIRCLE ( 'NONE', #4208, 0.2999999999999947153 ) ;
#1337 = CARTESIAN_POINT ( 'NONE',  ( 23.21374285137841298, 3.085791193308921265, 13.47995019114138415 ) ) ;
#1338 = CARTESIAN_POINT ( 'NONE',  ( -33.20000000000001705, -84.70000000000001705, 78.20000000000000284 ) ) ;
#1339 = DIRECTION ( 'NONE',  ( 0.000000000000000000, 1.000000000000000000, -0.000000000000000000 ) ) ;
#1340 = AXIS2_PLACEMENT_3D ( 'NONE', #21114, #15720, #19414 ) ;
#1341 = DIRECTION ( 'NONE',  ( 1.000000000000000000, 0.000000000000000000, 0.000000000000000000 ) ) ;
#1342 = CARTESIAN_POINT ( 'NONE',  ( 14.66174975910705847, 51.76873716947361714, 13.80000000000000071 ) ) ;
#1343 = AXIS2_PLACEMENT_3D ( 'NONE', #14433, #13924, #8589 ) ;
#1344 = EDGE_CURVE ( 'NONE', #8084, #10729, #15644, .T. ) ;
#1345 = VERTEX_POINT ( 'NONE', #9056 ) ;
#1346 = DIRECTION ( 'NONE',  ( 0.000000000000000000, 0.000000000000000000, 1.000000000000000000 ) ) ;
#1347 = ORIENTED_EDGE ( 'NONE', *, *, #20274, .T. ) ;
#1348 = CARTESIAN_POINT ( 'NONE',  ( 1.724728116533979838, 43.31054587065082728, 45.71679706732590631 ) ) ;
#1349 = CARTESIAN_POINT ( 'NONE',  ( 4.127054932750481520, 32.93424481021354921, 68.00000000000000000 ) ) ;
#1350 = VERTEX_POINT ( 'NONE', #19125 ) ;
#1351 = EDGE_LOOP ( 'NONE', ( #16475, #826, #15426, #17574 ) ) ;
#1352 = CARTESIAN_POINT ( 'NONE',  ( -1.824728116533986810, 43.26054587065083012, 49.66679706732590915 ) ) ;
#1353 =( NAMED_UNIT ( * ) SI_UNIT ( $, .STERADIAN. ) SOLID_ANGLE_UNIT ( ) );
#1354 = CIRCLE ( 'NONE', #4950, 0.2500000000000002220 ) ;
#1355 = CIRCLE ( 'NONE', #14930, 0.2500000000000002220 ) ;
#1356 = FILL_AREA_STYLE_COLOUR ( '', #5740 ) ;
#1357 = VERTEX_POINT ( 'NONE', #14302 ) ;
#1358 = ORIENTED_EDGE ( 'NONE', *, *, #2520, .T. ) ;
#1359 = CIRCLE ( 'NONE', #12420, 0.04999999999999991257 ) ;
#1360 = AXIS2_PLACEMENT_3D ( 'NONE', #12287, #19259, #334 ) ;
#1361 = ORIENTED_EDGE ( 'NONE', *, *, #9673, .F. ) ;
#1362 = AXIS2_PLACEMENT_3D ( 'NONE', #3889, #499, #10709 ) ;
#1363 = EDGE_CURVE ( 'NONE', #15493, #16055, #6509, .T. ) ;
#1364 = DIRECTION ( 'NONE',  ( 0.000000000000000000, 0.000000000000000000, -1.000000000000000000 ) ) ;
#1365 = ADVANCED_FACE ( 'NONE', ( #321 ), #10838, .T. ) ;
#1366 = DIRECTION ( 'NONE',  ( -0.000000000000000000, 0.000000000000000000, 1.000000000000000000 ) ) ;
#1367 = ORIENTED_EDGE ( 'NONE', *, *, #9430, .F. ) ;
#1368 =( NAMED_UNIT ( * ) PLANE_ANGLE_UNIT ( ) SI_UNIT ( $, .RADIAN. ) );
#1369 = CARTESIAN_POINT ( 'NONE',  ( -23.02398829872513986, 3.395586890286275139, 13.79999998301280328 ) ) ;
#1370 = DIRECTION ( 'NONE',  ( -0.000000000000000000, 1.000000000000000000, 0.000000000000000000 ) ) ;
#1371 = AXIS2_PLACEMENT_3D ( 'NONE', #15553, #19050, #10536 ) ;
#1372 = CARTESIAN_POINT ( 'NONE',  ( 25.37540678000427263, 67.54634676501045476, 7.500000000000000000 ) ) ;
#1373 = FACE_OUTER_BOUND ( 'NONE', #21577, .T. ) ;
#1374 = TOROIDAL_SURFACE ( 'NONE', #289, 0.05000000000000000278, 0.05000000000000000278 ) ;
#1375 = ORIENTED_EDGE ( 'NONE', *, *, #15709, .F. ) ;
#1376 = ORIENTED_EDGE ( 'NONE', *, *, #8385, .F. ) ;
#1377 = ORIENTED_EDGE ( 'NONE', *, *, #1011, .T. ) ;
#1378 = CARTESIAN_POINT ( 'NONE',  ( 4.127054932750481520, -32.93424481021354921, 42.50000000000000000 ) ) ;
#1379 = VECTOR ( 'NONE', #19012, 1000.000000000000000 ) ;
#1380 = LINE ( 'NONE', #5085, #11383 ) ;
#1381 = EDGE_LOOP ( 'NONE', ( #13518, #9293, #4886, #7780, #1024 ) ) ;
#1382 = EDGE_CURVE ( 'NONE', #21314, #14107, #19714, .T. ) ;
#1383 = ORIENTED_EDGE ( 'NONE', *, *, #17832, .T. ) ;
#1384 = DIRECTION ( 'NONE',  ( -0.000000000000000000, -0.000000000000000000, -1.000000000000000000 ) ) ;
#1385 = LINE ( 'NONE', #2966, #21696 ) ;
#1386 = EDGE_CURVE ( 'NONE', #8703, #5841, #2450, .T. ) ;
#1387 = ADVANCED_FACE ( 'NONE', ( #9278 ), #2115, .F. ) ;
#1388 = LINE ( 'NONE', #13685, #15292 ) ;
#1389 = AXIS2_PLACEMENT_3D ( 'NONE', #8012, #11570, #22120 ) ;
#1390 = LINE ( 'NONE', #3303, #21690 ) ;
#1391 = ORIENTED_EDGE ( 'NONE', *, *, #8160, .T. ) ;
#1392 = DIRECTION ( 'NONE',  ( -1.000000000000000000, -0.000000000000000000, 2.388292521039847891E-16 ) ) ;
#1393 = DIRECTION ( 'NONE',  ( 0.000000000000000000, 0.000000000000000000, 1.000000000000000000 ) ) ;
#1394 = PLANE ( 'NONE',  #5062 ) ;
#1395 = EDGE_LOOP ( 'NONE', ( #10162, #19516, #12645, #8970 ) ) ;
#1396 = CARTESIAN_POINT ( 'NONE',  ( 1.724728116533979616, 43.31054587065082728, 31.80876104995653719 ) ) ;
#1397 = CYLINDRICAL_SURFACE ( 'NONE', #12672, 0.5000000000000004441 ) ;
#1398 = VERTEX_POINT ( 'NONE', #3692 ) ;
#1399 = DIRECTION ( 'NONE',  ( -1.000000000000000000, -0.000000000000000000, -0.000000000000000000 ) ) ;
#1400 = LINE ( 'NONE', #13265, #15573 ) ;
#1401 = VERTEX_POINT ( 'NONE', #5385 ) ;
#1402 = ORIENTED_EDGE ( 'NONE', *, *, #5701, .F. ) ;
#1403 = ORIENTED_EDGE ( 'NONE', *, *, #10168, .F. ) ;
#1404 = DIRECTION ( 'NONE',  ( -4.336808689941893885E-15, 0.000000000000000000, 1.000000000000000000 ) ) ;
#1405 = EDGE_CURVE ( 'NONE', #13059, #10497, #3111, .T. ) ;
#1406 = CARTESIAN_POINT ( 'NONE',  ( 25.37540678000427263, 69.04634676501045476, 3.500000000000000000 ) ) ;
#1407 = AXIS2_PLACEMENT_3D ( 'NONE', #12272, #5493, #19122 ) ;
#1408 = AXIS2_PLACEMENT_3D ( 'NONE', #17856, #6239, #16165 ) ;
#1409 = TOROIDAL_SURFACE ( 'NONE', #13907, 5.299999999999999822, 0.2999999999999999889 ) ;
#1410 = EDGE_LOOP ( 'NONE', ( #5696, #6989, #820, #17040 ) ) ;
#1411 = CARTESIAN_POINT ( 'NONE',  ( -1.724728116533986721, 43.26054587065083012, 31.80876104995653719 ) ) ;
#1412 = VERTEX_POINT ( 'NONE', #8839 ) ;
#1413 = ORIENTED_EDGE ( 'NONE', *, *, #7285, .F. ) ;
#1414 = LINE ( 'NONE', #10047, #349 ) ;
#1415 = ADVANCED_FACE ( 'NONE', ( #13965 ), #426, .T. ) ;
#1416 = EDGE_CURVE ( 'NONE', #4773, #1863, #19197, .T. ) ;
#1417 = DIRECTION ( 'NONE',  ( 1.000000000000000000, 8.881784197001254296E-16, 0.000000000000000000 ) ) ;
#1418 = CARTESIAN_POINT ( 'NONE',  ( 29.13662752439705272, 5.000000000000000000, 7.200000000000000178 ) ) ;
#1419 = EDGE_CURVE ( 'NONE', #19294, #9791, #4572, .T. ) ;
#1420 = DIRECTION ( 'NONE',  ( -1.224646799147353207E-16, -0.000000000000000000, -1.000000000000000000 ) ) ;
#1421 = DIRECTION ( 'NONE',  ( -0.000000000000000000, -0.000000000000000000, -1.000000000000000000 ) ) ;
#1422 = CARTESIAN_POINT ( 'NONE',  ( 25.37540678000427263, 63.74634676501045050, 7.799999999999999822 ) ) ;
#1423 = LINE ( 'NONE', #6492, #13524 ) ;
#1424 = AXIS2_PLACEMENT_3D ( 'NONE', #21915, #18540, #11812 ) ;
#1425 = AXIS2_PLACEMENT_3D ( 'NONE', #20226, #4902, #18546 ) ;
#1426 = STYLED_ITEM ( 'NONE', ( #4292 ), #20456 ) ;
#1427 = CARTESIAN_POINT ( 'NONE',  ( 33.19999999999999574, 84.70000000000001705, 78.20000000000000284 ) ) ;
#1428 = PRODUCT_DEFINITION_SHAPE ( 'NONE', 'NONE',  #16121 ) ;
#1429 = CARTESIAN_POINT ( 'NONE',  ( -8.641460742840918030, 32.93424481021354921, 68.00000000000000000 ) ) ;
#1430 = ORIENTED_EDGE ( 'NONE', *, *, #360, .F. ) ;
#1431 = CARTESIAN_POINT ( 'NONE',  ( 14.66174975910705847, 0.000000000000000000, 13.50000000000000000 ) ) ;
#1432 = DIRECTION ( 'NONE',  ( 8.673617379884034239E-17, 0.000000000000000000, -1.000000000000000000 ) ) ;
#1433 = ORIENTED_EDGE ( 'NONE', *, *, #13453, .T. ) ;
#1434 = DIRECTION ( 'NONE',  ( -1.000000000000000000, -0.000000000000000000, -0.000000000000000000 ) ) ;
#1435 = EDGE_CURVE ( 'NONE', #6865, #3984, #9487, .T. ) ;
#1436 = CARTESIAN_POINT ( 'NONE',  ( 1.724728116533979616, 43.26054587065083012, 39.80876104995653719 ) ) ;
#1437 = ORIENTED_EDGE ( 'NONE', *, *, #13979, .T. ) ;
#1438 = ORIENTED_EDGE ( 'NONE', *, *, #3254, .T. ) ;
#1439 = CARTESIAN_POINT ( 'NONE',  ( -29.13662752439705272, 0.000000000000000000, 7.200000000000000178 ) ) ;
#1440 = VECTOR ( 'NONE', #12854, 1000.000000000000000 ) ;
#1441 = AXIS2_PLACEMENT_3D ( 'NONE', #14874, #1218, #18243 ) ;
#1442 = EDGE_CURVE ( 'NONE', #6809, #18032, #16429, .T. ) ;
#1443 = DIRECTION ( 'NONE',  ( 1.000000000000000000, 0.000000000000000000, 0.000000000000000000 ) ) ;
#1444 = CARTESIAN_POINT ( 'NONE',  ( 1.774728116533979438, 42.36054587065083155, 31.80876104995653719 ) ) ;
#1445 = EDGE_CURVE ( 'NONE', #7686, #22008, #13837, .T. ) ;
#1446 = EDGE_CURVE ( 'NONE', #13557, #4089, #6159, .T. ) ;
#1447 = LINE ( 'NONE', #20377, #4215 ) ;
#1448 = DIRECTION ( 'NONE',  ( 0.000000000000000000, 0.000000000000000000, -1.000000000000000000 ) ) ;
#1449 = CARTESIAN_POINT ( 'NONE',  ( 25.37540678000427263, -63.74634676501045050, 13.50000000000000000 ) ) ;
#1450 = CARTESIAN_POINT ( 'NONE',  ( 1.824728116533979705, 43.26054587065083012, 45.66679706732590205 ) ) ;
#1451 = AXIS2_PLACEMENT_3D ( 'NONE', #16177, #14735, #7698 ) ;
#1452 = FACE_OUTER_BOUND ( 'NONE', #11053, .T. ) ;
#1453 = CARTESIAN_POINT ( 'NONE',  ( -14.90262738048940960, -52.32122554936407255, 13.50000000000000000 ) ) ;
#1454 = DIRECTION ( 'NONE',  ( 0.000000000000000000, 0.000000000000000000, -1.000000000000000000 ) ) ;
#1455 = VERTEX_POINT ( 'NONE', #6264 ) ;
#1456 = EDGE_CURVE ( 'NONE', #11318, #1170, #16296, .T. ) ;
#1457 = CARTESIAN_POINT ( 'NONE',  ( -20.58855031337657593, 86.74083381065993592, 68.50000000000000000 ) ) ;
#1458 = VERTEX_POINT ( 'NONE', #979 ) ;
#1459 = CARTESIAN_POINT ( 'NONE',  ( -15.95292532278785913, -32.11873716947361856, 109.6002446535588319 ) ) ;
#1460 = VERTEX_POINT ( 'NONE', #862 ) ;
#1461 = ORIENTED_EDGE ( 'NONE', *, *, #16756, .T. ) ;
#1462 = DIRECTION ( 'NONE',  ( -0.000000000000000000, -0.000000000000000000, -1.000000000000000000 ) ) ;
#1463 = DIRECTION ( 'NONE',  ( 1.000000000000000000, 0.000000000000000000, 0.000000000000000000 ) ) ;
#1464 = EDGE_CURVE ( 'NONE', #19117, #4642, #11501, .T. ) ;
#1465 = PRESENTATION_LAYER_ASSIGNMENT (  '', '', ( #19036 ) ) ;
#1466 = ORIENTED_EDGE ( 'NONE', *, *, #22110, .F. ) ;
#1467 = TOROIDAL_SURFACE ( 'NONE', #1115, 1.300000000000000044, 0.2999999999999999889 ) ;
#1468 = SURFACE_STYLE_USAGE ( .BOTH. , #3490 ) ;
#1469 = ORIENTED_EDGE ( 'NONE', *, *, #3727, .F. ) ;
#1470 = ORIENTED_EDGE ( 'NONE', *, *, #6942, .T. ) ;
#1471 = AXIS2_PLACEMENT_3D ( 'NONE', #5011, #10148, #16962 ) ;
#1472 = EDGE_LOOP ( 'NONE', ( #11225, #14748 ) ) ;
#1473 = EDGE_CURVE ( 'NONE', #16854, #225, #12713, .T. ) ;
#1474 = CARTESIAN_POINT ( 'NONE',  ( -35.00000000000000000, 70.29999999999999716, 0.000000000000000000 ) ) ;
#1475 = DIRECTION ( 'NONE',  ( 0.000000000000000000, 1.000000000000000000, 0.000000000000000000 ) ) ;
#1476 = DIRECTION ( 'NONE',  ( -1.000000000000000000, 0.000000000000000000, 0.000000000000000000 ) ) ;
#1477 = DIRECTION ( 'NONE',  ( 0.000000000000000000, 0.000000000000000000, 1.000000000000000000 ) ) ;
#1478 = EDGE_LOOP ( 'NONE', ( #9469, #21640, #460, #2424 ) ) ;
#1479 = CARTESIAN_POINT ( 'NONE',  ( -21.71259690522456154, 45.22582864897715638, 13.75000000000000000 ) ) ;
#1480 = VECTOR ( 'NONE', #16480, 1000.000000000000000 ) ;
#1481 = DIRECTION ( 'NONE',  ( 1.000000000000000000, 0.000000000000000000, 0.000000000000000000 ) ) ;
#1482 = AXIS2_PLACEMENT_3D ( 'NONE', #20081, #19847, #12997 ) ;
#1483 = CARTESIAN_POINT ( 'NONE',  ( -1.724728116533986721, 42.36054587065083155, 35.80876104995653009 ) ) ;
#1484 = DIRECTION ( 'NONE',  ( 1.000000000000000000, 0.000000000000000000, 0.000000000000000000 ) ) ;
#1485 = CARTESIAN_POINT ( 'NONE',  ( 28.57540678000427548, -63.74634676501045050, 13.50000000000000000 ) ) ;
#1486 = VERTEX_POINT ( 'NONE', #9616 ) ;
#1487 = ORIENTED_EDGE ( 'NONE', *, *, #14223, .F. ) ;
#1488 = VERTEX_POINT ( 'NONE', #4244 ) ;
#1489 = CARTESIAN_POINT ( 'NONE',  ( 30.19999999999999574, 69.70000000000000284, 0.3000000000000033751 ) ) ;
#1491 = EDGE_CURVE ( 'NONE', #9271, #2915, #21371, .T. ) ;
#1490 = FACE_OUTER_BOUND ( 'NONE', #3204, .T. ) ;
#1492 = ORIENTED_EDGE ( 'NONE', *, *, #3274, .F. ) ;
#1493 = EDGE_CURVE ( 'NONE', #13584, #6556, #956, .T. ) ;
#1494 = EDGE_CURVE ( 'NONE', #8747, #18098, #11392, .T. ) ;
#1495 = CIRCLE ( 'NONE', #8997, 0.2999999999999999334 ) ;
#1496 = DIRECTION ( 'NONE',  ( 0.000000000000000000, 1.000000000000000000, 0.000000000000000000 ) ) ;
#1497 = CIRCLE ( 'NONE', #4366, 5.000000000000004441 ) ;
#1498 = AXIS2_PLACEMENT_3D ( 'NONE', #18426, #4450, #21813 ) ;
#1499 = ORIENTED_EDGE ( 'NONE', *, *, #20702, .T. ) ;
#1500 = DIRECTION ( 'NONE',  ( 1.000000000000000000, 0.000000000000000000, 0.000000000000000000 ) ) ;
#1501 = CARTESIAN_POINT ( 'NONE',  ( 29.69597781366221767, 25.99124249474150972, 68.75000000000000000 ) ) ;
#1502 = FACE_OUTER_BOUND ( 'NONE', #17458, .T. ) ;
#1503 = ORIENTED_EDGE ( 'NONE', *, *, #6884, .F. ) ;
#1504 = DIRECTION ( 'NONE',  ( 1.000000000000000000, 0.000000000000000000, 0.000000000000000000 ) ) ;
#1505 = FACE_OUTER_BOUND ( 'NONE', #18436, .T. ) ;
#1506 = DIRECTION ( 'NONE',  ( 0.000000000000000000, 0.000000000000000000, -1.000000000000000000 ) ) ;
#1507 = LINE ( 'NONE', #21998, #12637 ) ;
#1508 = ORIENTED_EDGE ( 'NONE', *, *, #15463, .F. ) ;
#1509 = EDGE_CURVE ( 'NONE', #16343, #16814, #13466, .T. ) ;
#1510 = DIRECTION ( 'NONE',  ( 1.000000000000000000, 0.000000000000000000, 0.000000000000000000 ) ) ;
#1511 = DIRECTION ( 'NONE',  ( -1.000000000000000000, 0.000000000000000000, 0.000000000000000000 ) ) ;
#1512 = CIRCLE ( 'NONE', #791, 0.2500000000000002220 ) ;
#1513 = VERTEX_POINT ( 'NONE', #21489 ) ;
#1514 = VECTOR ( 'NONE', #11137, 1000.000000000000000 ) ;
#1515 = ORIENTED_EDGE ( 'NONE', *, *, #20411, .T. ) ;
#1516 = VERTEX_POINT ( 'NONE', #14401 ) ;
#1517 = ORIENTED_EDGE ( 'NONE', *, *, #9821, .F. ) ;
#1518 = FACE_OUTER_BOUND ( 'NONE', #13221, .T. ) ;
#1519 = ADVANCED_FACE ( 'NONE', ( #13180 ), #19792, .T. ) ;
#1520 = DIRECTION ( 'NONE',  ( 0.000000000000000000, 0.000000000000000000, 1.000000000000000000 ) ) ;
#1521 = ORIENTED_EDGE ( 'NONE', *, *, #20493, .F. ) ;
#1522 = PLANE ( 'NONE',  #13487 ) ;
#1523 = AXIS2_PLACEMENT_3D ( 'NONE', #13116, #19968, #4632 ) ;
#1524 = ORIENTED_EDGE ( 'NONE', *, *, #18572, .F. ) ;
#1525 = VERTEX_POINT ( 'NONE', #19910 ) ;
#1526 = CARTESIAN_POINT ( 'NONE',  ( -28.87540678000427619, 6.494748934539263274, 13.19999999999999929 ) ) ;
#1527 = VERTEX_POINT ( 'NONE', #18221 ) ;
#1528 = FACE_OUTER_BOUND ( 'NONE', #18608, .T. ) ;
#1529 = CARTESIAN_POINT ( 'NONE',  ( -17.95292532278785913, -38.74634676501045760, 13.99999999999999822 ) ) ;
#1530 = DIRECTION ( 'NONE',  ( -0.000000000000000000, -0.000000000000000000, -1.000000000000000000 ) ) ;
#1531 = LINE ( 'NONE', #18656, #1982 ) ;
#1532 = CARTESIAN_POINT ( 'NONE',  ( 14.71174975910705740, 50.19799549595485644, 13.50000000000000000 ) ) ;
#1533 = DIRECTION ( 'NONE',  ( -1.000000000000000000, 3.009265538104883829E-28, -4.336808689941893885E-15 ) ) ;
#1534 = DIRECTION ( 'NONE',  ( 0.000000000000000000, 0.000000000000000000, -1.000000000000000000 ) ) ;
#1535 = VERTEX_POINT ( 'NONE', #21704 ) ;
#1536 = CARTESIAN_POINT ( 'NONE',  ( -29.13662752439705272, 0.000000000000000000, 7.500000000000000000 ) ) ;
#1537 = ORIENTED_EDGE ( 'NONE', *, *, #13957, .T. ) ;
#1538 = DIRECTION ( 'NONE',  ( 0.000000000000000000, -0.000000000000000000, 1.000000000000000000 ) ) ;
#1539 = ADVANCED_FACE ( 'NONE', ( #2559 ), #20026, .T. ) ;
#1540 = DIRECTION ( 'NONE',  ( 2.105859220307292343E-16, -1.000000000000000000, 0.000000000000000000 ) ) ;
#1541 = ORIENTED_EDGE ( 'NONE', *, *, #6935, .T. ) ;
#1542 = EDGE_CURVE ( 'NONE', #12877, #4113, #9543, .T. ) ;
#1543 = ORIENTED_EDGE ( 'NONE', *, *, #18336, .T. ) ;
#1544 = DIRECTION ( 'NONE',  ( -1.000000000000000000, 0.000000000000000000, 0.000000000000000000 ) ) ;
#1545 = VERTEX_POINT ( 'NONE', #11824 ) ;
#1546 = ADVANCED_FACE ( 'NONE', ( #15080 ), #4794, .T. ) ;
#1547 = CARTESIAN_POINT ( 'NONE',  ( 1.774728116533979660, 43.31054587065082728, 37.66679706732590915 ) ) ;
#1548 = ORIENTED_EDGE ( 'NONE', *, *, #21487, .T. ) ;
#1549 = PRESENTATION_LAYER_ASSIGNMENT (  '', '', ( #7640 ) ) ;
#1550 = CARTESIAN_POINT ( 'NONE',  ( 0.000000000000000000, -85.00000000000000000, 78.79999999999999716 ) ) ;
#1551 = CARTESIAN_POINT ( 'NONE',  ( 30.37540678000427619, 63.74634676501045050, 7.200000000000000178 ) ) ;
#1552 = DIRECTION ( 'NONE',  ( 0.000000000000000000, 0.000000000000000000, 1.000000000000000000 ) ) ;
#1553 = EDGE_CURVE ( 'NONE', #20330, #9891, #8489, .T. ) ;
#1554 = DIRECTION ( 'NONE',  ( -0.000000000000000000, 1.000000000000000000, -0.000000000000000000 ) ) ;
#1555 = LINE ( 'NONE', #1450, #18263 ) ;
#1556 = AXIS2_PLACEMENT_3D ( 'NONE', #7359, #14052, #7035 ) ;
#1557 = DIRECTION ( 'NONE',  ( 0.000000000000000000, -0.000000000000000000, -1.000000000000000000 ) ) ;
#1558 = CARTESIAN_POINT ( 'NONE',  ( 3.127054932750481964, -32.61873716947361856, 68.50000000000000000 ) ) ;
#1559 = CARTESIAN_POINT ( 'NONE',  ( -25.37540678000427263, 63.74634676501045050, 7.500000000000000000 ) ) ;
#1560 =( REPRESENTATION_RELATIONSHIP ('NONE','NONE', #561, #10840 ) REPRESENTATION_RELATIONSHIP_WITH_TRANSFORMATION ( #12728 )SHAPE_REPRESENTATION_RELATIONSHIP( ) );
#1561 = EDGE_CURVE ( 'NONE', #11695, #9706, #12392, .T. ) ;
#1562 = ORIENTED_EDGE ( 'NONE', *, *, #20368, .T. ) ;
#1563 = EDGE_CURVE ( 'NONE', #15847, #17106, #20130, .T. ) ;
#1564 = DIRECTION ( 'NONE',  ( 0.000000000000000000, 0.000000000000000000, 1.000000000000000000 ) ) ;
#1565 = ORIENTED_EDGE ( 'NONE', *, *, #1936, .F. ) ;
#1566 = CARTESIAN_POINT ( 'NONE',  ( -15.21174975910705207, 51.61873716947361856, 14.00000000000000000 ) ) ;
#1567 = VECTOR ( 'NONE', #2688, 1000.000000000000000 ) ;
#1568 = ADVANCED_FACE ( 'NONE', ( #13623 ), #12382, .T. ) ;
#1569 = CARTESIAN_POINT ( 'NONE',  ( -21.67365502786443088, 45.72430987248279166, 68.25000000000000000 ) ) ;
#1570 = ORIENTED_EDGE ( 'NONE', *, *, #6982, .T. ) ;
#1571 = CIRCLE ( 'NONE', #19809, 1.999999999999991340 ) ;
#1572 = ORIENTED_EDGE ( 'NONE', *, *, #1589, .F. ) ;
#1573 = CARTESIAN_POINT ( 'NONE',  ( 9.141460742840918030, 32.93424481021354921, 13.50000000000000000 ) ) ;
#1574 = EDGE_CURVE ( 'NONE', #9296, #17196, #9899, .T. ) ;
#1575 = SHAPE_DEFINITION_REPRESENTATION ( #11783, #561 ) ;
#1576 = ORIENTED_EDGE ( 'NONE', *, *, #18839, .F. ) ;
#1577 = VERTEX_POINT ( 'NONE', #6831 ) ;
#1578 = EDGE_LOOP ( 'NONE', ( #13780, #306, #5689, #3602 ) ) ;
#1579 = DIRECTION ( 'NONE',  ( 0.000000000000000000, 0.000000000000000000, 1.000000000000000000 ) ) ;
#1580 = EDGE_CURVE ( 'NONE', #9271, #21431, #2754, .T. ) ;
#1581 = CARTESIAN_POINT ( 'NONE',  ( 14.66174954729678248, -51.84624528035402591, 13.50000000000000000 ) ) ;
#1582 = DIRECTION ( 'NONE',  ( 0.000000000000000000, -1.000000000000000000, 0.000000000000000000 ) ) ;
#1583 = EDGE_LOOP ( 'NONE', ( #4955, #12650, #10583, #13460 ) ) ;
#1584 = DIRECTION ( 'NONE',  ( 0.000000000000000000, -0.000000000000000000, 1.000000000000000000 ) ) ;
#1585 = CARTESIAN_POINT ( 'NONE',  ( -23.02398829872513986, 3.528912754968630328, 13.50000000000000000 ) ) ;
#1586 = FACE_OUTER_BOUND ( 'NONE', #14167, .T. ) ;
#1587 = DIRECTION ( 'NONE',  ( 0.000000000000000000, 0.000000000000000000, 1.000000000000000000 ) ) ;
#1588 = CARTESIAN_POINT ( 'NONE',  ( -29.50000000000002132, 0.000000000000000000, 1.500000000000000000 ) ) ;
#1589 = EDGE_CURVE ( 'NONE', #5063, #20665, #1680, .T. ) ;
#1590 = VERTEX_POINT ( 'NONE', #16974 ) ;
#1591 = VERTEX_POINT ( 'NONE', #18429 ) ;
#1592 = VERTEX_POINT ( 'NONE', #1643 ) ;
#1593 = CARTESIAN_POINT ( 'NONE',  ( -25.37540678000427263, 66.94634676501046044, 13.50000000000000000 ) ) ;
#1594 = EDGE_CURVE ( 'NONE', #2890, #7001, #6711, .T. ) ;
#1595 = DIRECTION ( 'NONE',  ( 1.000000000000000000, 0.000000000000000000, -0.000000000000000000 ) ) ;
#1596 = EDGE_LOOP ( 'NONE', ( #21372, #3792, #6050, #3016 ) ) ;
#1597 = VECTOR ( 'NONE', #3258, 1000.000000000000000 ) ;
#1598 = CARTESIAN_POINT ( 'NONE',  ( 14.97552947837228388, -51.92046840034491595, 13.84856038353110463 ) ) ;
#1599 = AXIS2_PLACEMENT_3D ( 'NONE', #4156, #7419, #17803 ) ;
#1600 = EDGE_LOOP ( 'NONE', ( #527, #18675, #6558, #19357 ) ) ;
#1601 = DIRECTION ( 'NONE',  ( 0.000000000000000000, 0.000000000000000000, 1.000000000000000000 ) ) ;
#1602 = LINE ( 'NONE', #6997, #7757 ) ;
#1603 = DIRECTION ( 'NONE',  ( -0.000000000000000000, -1.000000000000000000, -0.000000000000000000 ) ) ;
#1604 = DIRECTION ( 'NONE',  ( 0.000000000000000000, 0.000000000000000000, 1.000000000000000000 ) ) ;
#1605 = ORIENTED_EDGE ( 'NONE', *, *, #6167, .T. ) ;
#1606 = CYLINDRICAL_SURFACE ( 'NONE', #7394, 0.05000000000000143219 ) ;
#1607 = CARTESIAN_POINT ( 'NONE',  ( 34.39999999999998437, -84.70000000000001705, 0.6000000000000041966 ) ) ;
#1608 = ADVANCED_FACE ( 'NONE', ( #5133 ), #18549, .T. ) ;
#1609 = DIRECTION ( 'NONE',  ( 1.000000000000000000, 0.000000000000000000, 0.000000000000000000 ) ) ;
#1610 = EDGE_CURVE ( 'NONE', #17480, #20423, #12044, .T. ) ;
#1611 = DIRECTION ( 'NONE',  ( 1.000000000000000000, 0.000000000000000000, 0.000000000000000000 ) ) ;
#1612 = CARTESIAN_POINT ( 'NONE',  ( 4.127054932750481520, -32.93424481021354921, 68.00000000000000000 ) ) ;
#1613 = ORIENTED_EDGE ( 'NONE', *, *, #17580, .F. ) ;
#1614 = FACE_OUTER_BOUND ( 'NONE', #8727, .T. ) ;
#1615 = AXIS2_PLACEMENT_3D ( 'NONE', #3649, #19187, #15489 ) ;
#1616 = VECTOR ( 'NONE', #20133, 1000.000000000000000 ) ;
#1617 = ORIENTED_EDGE ( 'NONE', *, *, #10800, .F. ) ;
#1618 = CARTESIAN_POINT ( 'NONE',  ( -8.638906393579159015, 41.58710221366784054, 69.00503344894293889 ) ) ;
#1619 = CARTESIAN_POINT ( 'NONE',  ( -9.178906393579033818, 42.46645089659918426, 1067.751649863784678 ) ) ;
#1620 = EDGE_LOOP ( 'NONE', ( #21323, #12891, #18593, #14003, #17914 ) ) ;
#1621 = VERTEX_POINT ( 'NONE', #3232 ) ;
#1622 = EDGE_LOOP ( 'NONE', ( #3180, #10516, #20398, #12726 ) ) ;
#1623 = DIRECTION ( 'NONE',  ( 3.052134192567367925E-16, -1.000000000000000000, 0.000000000000000000 ) ) ;
#1624 = EDGE_CURVE ( 'NONE', #21684, #16460, #13108, .T. ) ;
#1625 = CARTESIAN_POINT ( 'NONE',  ( 29.05186365738250842, 0.05288320938007240457, 0.2999999999999947153 ) ) ;
#1626 = ORIENTED_EDGE ( 'NONE', *, *, #21936, .F. ) ;
#1627 = DIRECTION ( 'NONE',  ( 1.000000000000000000, 0.000000000000000000, -0.000000000000000000 ) ) ;
#1628 = AXIS2_PLACEMENT_3D ( 'NONE', #10318, #1684, #17130 ) ;
#1629 = EDGE_LOOP ( 'NONE', ( #15851, #6021, #13552, #4373 ) ) ;
#1630 = DIRECTION ( 'NONE',  ( -1.000000000000000000, 0.000000000000000000, 0.000000000000000000 ) ) ;
#1631 = AXIS2_PLACEMENT_3D ( 'NONE', #8064, #16210, #18239 ) ;
#1632 = AXIS2_PLACEMENT_3D ( 'NONE', #13798, #12228, #15810 ) ;
#1633 = AXIS2_PLACEMENT_3D ( 'NONE', #21783, #6340, #14711 ) ;
#1634 = ORIENTED_EDGE ( 'NONE', *, *, #15888, .F. ) ;
#1635 = CARTESIAN_POINT ( 'NONE',  ( -1.724728116533986721, 42.31054587065082728, 47.80876104995653719 ) ) ;
#1636 = CARTESIAN_POINT ( 'NONE',  ( -14.96174975910705207, 51.86873716947361856, 13.05380965755523448 ) ) ;
#1637 = DIRECTION ( 'NONE',  ( 1.000000000000000000, 0.000000000000000000, 0.000000000000000000 ) ) ;
#1638 = CARTESIAN_POINT ( 'NONE',  ( 17.45292532278785913, -38.74634676501045760, 14.00000000000000000 ) ) ;
#1639 = VERTEX_POINT ( 'NONE', #11933 ) ;
#1640 = PLANE ( 'NONE',  #17722 ) ;
#1641 = CARTESIAN_POINT ( 'NONE',  ( -32.47706987357031494, 83.66206381164209915, 13.50000000000000000 ) ) ;
#1642 = EDGE_CURVE ( 'NONE', #573, #8339, #21817, .T. ) ;
#1643 = CARTESIAN_POINT ( 'NONE',  ( -19.85144383993102934, 42.46645089659918426, 13.49999999999999822 ) ) ;
#1644 = CARTESIAN_POINT ( 'NONE',  ( 0.000000000000000000, -68.74634676501045760, 7.500000000000000000 ) ) ;
#1645 = ORIENTED_EDGE ( 'NONE', *, *, #17349, .F. ) ;
#1646 = ADVANCED_FACE ( 'NONE', ( #18771 ), #22031, .T. ) ;
#1647 = VECTOR ( 'NONE', #20575, 1000.000000000000000 ) ;
#1648 = DIRECTION ( 'NONE',  ( 1.000000000000000000, -0.000000000000000000, 0.000000000000000000 ) ) ;
#1649 = CIRCLE ( 'NONE', #7021, 0.5000000000000004441 ) ;
#1650 = FACE_OUTER_BOUND ( 'NONE', #12109, .T. ) ;
#1651 = ORIENTED_EDGE ( 'NONE', *, *, #18989, .F. ) ;
#1652 = VECTOR ( 'NONE', #14016, 999.9999999999998863 ) ;
#1653 = PLANE ( 'NONE',  #3897 ) ;
#1654 = CARTESIAN_POINT ( 'NONE',  ( -21.67365502786443088, 45.72430987248279166, 13.74999999999999822 ) ) ;
#1655 = ORIENTED_EDGE ( 'NONE', *, *, #921, .T. ) ;
#1656 = DIRECTION ( 'NONE',  ( -2.107255972849994642E-16, 0.000000000000000000, -1.000000000000000000 ) ) ;
#1657 = VERTEX_POINT ( 'NONE', #3444 ) ;
#1658 = ADVANCED_FACE ( 'NONE', ( #10280 ), #20569, .T. ) ;
#1659 = AXIS2_PLACEMENT_3D ( 'NONE', #16500, #16597, #8011 ) ;
#1660 = AXIS2_PLACEMENT_3D ( 'NONE', #17749, #10927, #11370 ) ;
#1661 = CIRCLE ( 'NONE', #13445, 0.05000000000000143219 ) ;
#1662 = LINE ( 'NONE', #8506, #21026 ) ;
#1663 = ORIENTED_EDGE ( 'NONE', *, *, #11252, .T. ) ;
#1664 = DIRECTION ( 'NONE',  ( 0.000000000000000000, 0.000000000000000000, 1.000000000000000000 ) ) ;
#1665 = CIRCLE ( 'NONE', #6335, 0.3000000000000016542 ) ;
#1666 = DIRECTION ( 'NONE',  ( 1.000000000000000000, 0.000000000000000000, 0.000000000000000000 ) ) ;
#1667 = ADVANCED_FACE ( 'NONE', ( #8813 ), #506, .T. ) ;
#1668 = LINE ( 'NONE', #8292, #3144 ) ;
#1669 = EDGE_CURVE ( 'NONE', #12996, #1905, #11203, .T. ) ;
#1670 = FACE_OUTER_BOUND ( 'NONE', #11665, .T. ) ;
#1671 = DIRECTION ( 'NONE',  ( -0.000000000000000000, -0.000000000000000000, -1.000000000000000000 ) ) ;
#1672 = DIRECTION ( 'NONE',  ( 1.000000000000000000, 0.000000000000000000, 0.000000000000000000 ) ) ;
#1673 = CARTESIAN_POINT ( 'NONE',  ( -31.50000000000002132, -71.70000000000001705, 1.500000000000000000 ) ) ;
#1674 = AXIS2_PLACEMENT_3D ( 'NONE', #2266, #12548, #1931 ) ;
#1675 = CARTESIAN_POINT ( 'NONE',  ( -15.00548668436308830, -51.86811046850819906, 13.49999999999993072 ) ) ;
#1676 = CARTESIAN_POINT ( 'NONE',  ( -17.93704824106378837, 0.000000000000000000, 13.87500000000000000 ) ) ;
#1677 = VECTOR ( 'NONE', #16986, 1000.000000000000000 ) ;
#1678 = VECTOR ( 'NONE', #12334, 1000.000000000000000 ) ;
#1679 = ORIENTED_EDGE ( 'NONE', *, *, #9739, .F. ) ;
#1680 = CIRCLE ( 'NONE', #16314, 2.000000000000001776 ) ;
#1681 = CARTESIAN_POINT ( 'NONE',  ( -1.774728116533986766, 42.31054587065082728, 45.66679706732590205 ) ) ;
#1682 = LINE ( 'NONE', #8199, #17729 ) ;
#1683 = TOROIDAL_SURFACE ( 'NONE', #10279, 4.700000000000000178, 0.2999999999999999889 ) ;
#1684 = DIRECTION ( 'NONE',  ( 0.000000000000000000, 1.000000000000000000, 0.000000000000000000 ) ) ;
#1685 = ORIENTED_EDGE ( 'NONE', *, *, #21805, .T. ) ;
#1686 = CIRCLE ( 'NONE', #15965, 0.05000000000000143219 ) ;
#1687 = ORIENTED_EDGE ( 'NONE', *, *, #18273, .T. ) ;
#1688 = DIRECTION ( 'NONE',  ( 1.000000000000000000, 0.000000000000000000, 0.000000000000000000 ) ) ;
#1689 = DIRECTION ( 'NONE',  ( 1.000000000000000000, 0.000000000000000000, 0.000000000000000000 ) ) ;
#1690 = EDGE_CURVE ( 'NONE', #17214, #17444, #4426, .T. ) ;
#1691 = ORIENTED_EDGE ( 'NONE', *, *, #9386, .T. ) ;
#1692 = SHAPE_REPRESENTATION_RELATIONSHIP ( 'NONE' , 'NONE' ,  #9142, #45 ) ;
#1693 = ORIENTED_EDGE ( 'NONE', *, *, #2107, .T. ) ;
#1694 = CIRCLE ( 'NONE', #8845, 0.5000000000000000000 ) ;
#1695 = ORIENTED_EDGE ( 'NONE', *, *, #16338, .F. ) ;
#1696 = EDGE_CURVE ( 'NONE', #15684, #19966, #14784, .T. ) ;
#1697 = DIRECTION ( 'NONE',  ( 1.000000000000000000, 0.000000000000000000, -0.000000000000000000 ) ) ;
#1698 = CYLINDRICAL_SURFACE ( 'NONE', #249, 0.1000000000000028644 ) ;
#1699 = EDGE_CURVE ( 'NONE', #17937, #16591, #10715, .T. ) ;
#1700 = DIRECTION ( 'NONE',  ( 0.000000000000000000, 0.000000000000000000, -1.000000000000000000 ) ) ;
#1701 = AXIS2_PLACEMENT_3D ( 'NONE', #5084, #17154, #1713 ) ;
#1702 = DIRECTION ( 'NONE',  ( -0.9729678061520371513, -0.2309407893631869879, 0.000000000000000000 ) ) ;
#1703 = CIRCLE ( 'NONE', #8854, 0.6000000000000033085 ) ;
#1704 = DIRECTION ( 'NONE',  ( 1.224646799147353207E-16, 1.000000000000000000, 0.000000000000000000 ) ) ;
#1705 = FACE_OUTER_BOUND ( 'NONE', #14578, .T. ) ;
#1706 = CARTESIAN_POINT ( 'NONE',  ( 1.724728116533979616, 43.26054587065083012, 35.80876104995653009 ) ) ;
#1707 = CARTESIAN_POINT ( 'NONE',  ( -21.92816239687475743, 42.46645089659918426, 68.50000000000000000 ) ) ;
#1708 = ORIENTED_EDGE ( 'NONE', *, *, #9949, .F. ) ;
#1709 = CIRCLE ( 'NONE', #17792, 0.2500000000000002220 ) ;
#1710 = AXIS2_PLACEMENT_3D ( 'NONE', #19338, #13840, #5484 ) ;
#1711 = VERTEX_POINT ( 'NONE', #19218 ) ;
#1712 = EDGE_LOOP ( 'NONE', ( #78, #5706, #1361, #4255 ) ) ;
#1713 = DIRECTION ( 'NONE',  ( 0.000000000000000000, 0.000000000000000000, 1.000000000000000000 ) ) ;
#1714 =( NAMED_UNIT ( * ) SI_UNIT ( $, .STERADIAN. ) SOLID_ANGLE_UNIT ( ) );
#1715 = DIRECTION ( 'NONE',  ( 0.000000000000000000, 0.000000000000000000, 1.000000000000000000 ) ) ;
#1716 = ADVANCED_FACE ( 'NONE', ( #12152 ), #12476, .T. ) ;
#1717 = EDGE_LOOP ( 'NONE', ( #18901, #991, #21614, #15084 ) ) ;
#1718 = AXIS2_PLACEMENT_3D ( 'NONE', #16891, #21941, #6617 ) ;
#1719 = CARTESIAN_POINT ( 'NONE',  ( -18.22752199202934520, 0.000000000000000000, 13.79999999999999893 ) ) ;
#1720 = CIRCLE ( 'NONE', #7091, 0.5000000000000004441 ) ;
#1721 = EDGE_LOOP ( 'NONE', ( #21799, #2456, #14260, #10433 ) ) ;
#1722 = VECTOR ( 'NONE', #5893, 1000.000000000000000 ) ;
#1723 = ORIENTED_EDGE ( 'NONE', *, *, #6142, .F. ) ;
#1724 = DIRECTION ( 'NONE',  ( 0.000000000000000000, 0.000000000000000000, 1.000000000000000000 ) ) ;
#1725 = EDGE_CURVE ( 'NONE', #573, #15418, #7298, .T. ) ;
#1726 = CARTESIAN_POINT ( 'NONE',  ( 1.724728116533979616, 43.26054587065083012, 27.70876104995653577 ) ) ;
#1727 = ADVANCED_FACE ( 'NONE', ( #2200 ), #8014, .T. ) ;
#1728 = CIRCLE ( 'NONE', #3474, 0.05000000000000143219 ) ;
#1729 = AXIS2_PLACEMENT_3D ( 'NONE', #4229, #11047, #21355 ) ;
#1730 = CARTESIAN_POINT ( 'NONE',  ( 30.49999999999999645, -84.70000000000001705, 1.500000000000004885 ) ) ;
#1731 = ORIENTED_EDGE ( 'NONE', *, *, #21343, .F. ) ;
#1732 = CARTESIAN_POINT ( 'NONE',  ( 29.05186365738250842, 0.05288320938007240457, 1.500000000000000000 ) ) ;
#1733 = EDGE_CURVE ( 'NONE', #12990, #15862, #19803, .T. ) ;
#1734 = DIRECTION ( 'NONE',  ( 1.000000000000000000, 0.000000000000000000, 0.000000000000000000 ) ) ;
#1735 = FACE_OUTER_BOUND ( 'NONE', #6534, .T. ) ;
#1736 = AXIS2_PLACEMENT_3D ( 'NONE', #6597, #18548, #18659 ) ;
#1737 = CARTESIAN_POINT ( 'NONE',  ( 1.724728116533979616, 42.36054587065083155, 39.70876104995653577 ) ) ;
#1738 = PLANE ( 'NONE',  #21504 ) ;
#1739 = ORIENTED_EDGE ( 'NONE', *, *, #11285, .F. ) ;
#1740 = DIRECTION ( 'NONE',  ( -1.000000000000000000, 0.000000000000000000, 0.000000000000000000 ) ) ;
#1741 = CIRCLE ( 'NONE', #14234, 0.1000000000000028644 ) ;
#1742 = AXIS2_PLACEMENT_3D ( 'NONE', #14200, #3935, #8853 ) ;
#1743 = AXIS2_PLACEMENT_3D ( 'NONE', #12051, #18902, #3574 ) ;
#1744 = ORIENTED_EDGE ( 'NONE', *, *, #20998, .F. ) ;
#1745 = LINE ( 'NONE', #17176, #15044 ) ;
#1746 = CARTESIAN_POINT ( 'NONE',  ( -14.66174975910705136, 0.000000000000000000, 13.79999999999999893 ) ) ;
#1747 = LINE ( 'NONE', #20208, #20248 ) ;
#1748 = VERTEX_POINT ( 'NONE', #14157 ) ;
#1749 = ORIENTED_EDGE ( 'NONE', *, *, #8093, .F. ) ;
#1750 = VERTEX_POINT ( 'NONE', #20794 ) ;
#1751 = DIRECTION ( 'NONE',  ( -1.000000000000000000, 0.000000000000000000, -6.123233995736764803E-17 ) ) ;
#1752 = CARTESIAN_POINT ( 'NONE',  ( 30.79999999999999716, -84.70000000000001705, 0.3000000000000039857 ) ) ;
#1753 = DIRECTION ( 'NONE',  ( 0.000000000000000000, 1.000000000000000000, -0.000000000000000000 ) ) ;
#1754 = EDGE_LOOP ( 'NONE', ( #15471, #21587, #18670, #2197 ) ) ;
#1755 = LINE ( 'NONE', #8593, #12746 ) ;
#1756 = EDGE_CURVE ( 'NONE', #9468, #9603, #17995, .T. ) ;
#1757 = AXIS2_PLACEMENT_3D ( 'NONE', #15048, #11901, #14934 ) ;
#1758 = ORIENTED_EDGE ( 'NONE', *, *, #5831, .F. ) ;
#1759 = PLANE ( 'NONE',  #8228 ) ;
#1760 = AXIS2_PLACEMENT_3D ( 'NONE', #2119, #20920, #7386 ) ;
#1761 = ORIENTED_EDGE ( 'NONE', *, *, #533, .T. ) ;
#1762 = CARTESIAN_POINT ( 'NONE',  ( -23.02398829872513986, -3.528912754968629439, 13.50000000000000178 ) ) ;
#1763 = CARTESIAN_POINT ( 'NONE',  ( -17.95292532278785913, 0.000000000000000000, 13.99999999999999822 ) ) ;
#1764 = CARTESIAN_POINT ( 'NONE',  ( 29.69597781366221767, 56.94165929845684104, 68.75000000000000000 ) ) ;
#1765 = CARTESIAN_POINT ( 'NONE',  ( -14.37248138918699425, 42.46645089659917716, 70.50000000000000000 ) ) ;
#1766 = ORIENTED_EDGE ( 'NONE', *, *, #6121, .T. ) ;
#1767 = CARTESIAN_POINT ( 'NONE',  ( -29.50000000000002132, 0.000000000000000000, -150.0833101980363722 ) ) ;
#1768 = EDGE_CURVE ( 'NONE', #1239, #9810, #3359, .T. ) ;
#1769 = DIRECTION ( 'NONE',  ( 0.000000000000000000, -1.000000000000000000, 0.000000000000000000 ) ) ;
#1770 = DIRECTION ( 'NONE',  ( 0.000000000000000000, 0.000000000000000000, 1.000000000000000000 ) ) ;
#1771 = CARTESIAN_POINT ( 'NONE',  ( 33.49999999999998579, 85.00000000000000000, 80.00000000000000000 ) ) ;
#1772 = ORIENTED_EDGE ( 'NONE', *, *, #2131, .F. ) ;
#1773 = CARTESIAN_POINT ( 'NONE',  ( 15.95292532278785913, -52.39333383871510108, 13.50000000000000000 ) ) ;
#1774 = AXIS2_PLACEMENT_3D ( 'NONE', #13540, #8735, #8629 ) ;
#1775 = LINE ( 'NONE', #6943, #18074 ) ;
#1776 = EDGE_LOOP ( 'NONE', ( #13596, #2910, #20139, #21929 ) ) ;
#1777 = CARTESIAN_POINT ( 'NONE',  ( -14.96174975910705207, 32.10873716947361345, 68.25000000000000000 ) ) ;
#1778 = DIRECTION ( 'NONE',  ( 1.000000000000000000, 0.000000000000000000, 0.000000000000000000 ) ) ;
#1779 = ORIENTED_EDGE ( 'NONE', *, *, #20353, .T. ) ;
#1780 = VERTEX_POINT ( 'NONE', #15940 ) ;
#1781 = CARTESIAN_POINT ( 'NONE',  ( -29.13662752439705272, 5.000000000000000000, 3.799999999999999822 ) ) ;
#1782 = EDGE_CURVE ( 'NONE', #10170, #6971, #21129, .T. ) ;
#1783 = ORIENTED_EDGE ( 'NONE', *, *, #12823, .F. ) ;
#1784 = EDGE_CURVE ( 'NONE', #6525, #7145, #141, .T. ) ;
#1785 = PLANE ( 'NONE',  #4579 ) ;
#1786 = AXIS2_PLACEMENT_3D ( 'NONE', #17650, #3920, #10738 ) ;
#1787 = ORIENTED_EDGE ( 'NONE', *, *, #3300, .T. ) ;
#1788 = DIRECTION ( 'NONE',  ( 0.000000000000000000, 0.000000000000000000, 1.000000000000000000 ) ) ;
#1789 = VECTOR ( 'NONE', #8662, 1000.000000000000000 ) ;
#1790 = AXIS2_PLACEMENT_3D ( 'NONE', #5118, #16740, #10042 ) ;
#1791 = DIRECTION ( 'NONE',  ( -1.224646799147353207E-16, -1.000000000000000000, 0.000000000000000000 ) ) ;
#1792 = CARTESIAN_POINT ( 'NONE',  ( 34.99999999999999289, 84.70000000000001705, 79.39999999999999147 ) ) ;
#1793 = CARTESIAN_POINT ( 'NONE',  ( 1.724728116533978728, 43.31054587065082728, 37.71679706732590631 ) ) ;
#1794 = LINE ( 'NONE', #3143, #17287 ) ;
#1795 = CARTESIAN_POINT ( 'NONE',  ( -15.12826760881917387, -51.99271056040087302, 13.49999999999999822 ) ) ;
#1796 = EDGE_CURVE ( 'NONE', #9870, #14272, #2089, .T. ) ;
#1797 = AXIS2_PLACEMENT_3D ( 'NONE', #6787, #20531, #10233 ) ;
#1798 = VERTEX_POINT ( 'NONE', #20897 ) ;
#1799 = CARTESIAN_POINT ( 'NONE',  ( -1.724728116533986721, 43.31054587065082728, 53.66679706732590915 ) ) ;
#1800 = DIRECTION ( 'NONE',  ( -1.000000000000000000, 0.000000000000000000, 2.107255972849994642E-16 ) ) ;
#1801 = CIRCLE ( 'NONE', #14297, 0.2999999999999999334 ) ;
#1802 = PRODUCT_DEFINITION_SHAPE ( 'NONE', 'NONE',  #22165 ) ;
#1803 = CARTESIAN_POINT ( 'NONE',  ( -13.37248138918699425, 42.46645089659917716, 68.50000000000000000 ) ) ;
#1804 = DIRECTION ( 'NONE',  ( 0.000000000000000000, 0.000000000000000000, 1.000000000000000000 ) ) ;
#1805 = ORIENTED_EDGE ( 'NONE', *, *, #1553, .T. ) ;
#1806 = VERTEX_POINT ( 'NONE', #17300 ) ;
#1807 = CARTESIAN_POINT ( 'NONE',  ( -25.37540678000427263, 63.74634676501045050, 13.19999999999999929 ) ) ;
#1808 = APPLICATION_PROTOCOL_DEFINITION ( 'draft international standard', 'automotive_design', 1998, #6598 ) ;
#1809 = EDGE_CURVE ( 'NONE', #10275, #10408, #8361, .T. ) ;
#1810 = ORIENTED_EDGE ( 'NONE', *, *, #19090, .T. ) ;
#1811 = ORIENTED_EDGE ( 'NONE', *, *, #3064, .T. ) ;
#1812 = ORIENTED_EDGE ( 'NONE', *, *, #3472, .T. ) ;
#1813 = VERTEX_POINT ( 'NONE', #8924 ) ;
#1814 = AXIS2_PLACEMENT_3D ( 'NONE', #2978, #4432, #955 ) ;
#1815 = CARTESIAN_POINT ( 'NONE',  ( 0.000000000000000000, 67.54634676501045476, 7.799999999999999822 ) ) ;
#1816 = DIRECTION ( 'NONE',  ( 0.000000000000000000, -1.000000000000000000, 0.000000000000000000 ) ) ;
#1817 = DIRECTION ( 'NONE',  ( -1.000000000000000000, -0.000000000000000000, 2.388292521039847891E-16 ) ) ;
#1818 = PLANE ( 'NONE',  #9306 ) ;
#1819 = ADVANCED_FACE ( 'NONE', ( #403 ), #13830, .T. ) ;
#1820 = DIRECTION ( 'NONE',  ( 0.000000000000000000, 1.000000000000000000, 0.000000000000000000 ) ) ;
#1821 = CARTESIAN_POINT ( 'NONE',  ( -1.824728116533986810, 42.36054587065083155, 33.71679706732589921 ) ) ;
#1822 = CARTESIAN_POINT ( 'NONE',  ( 23.04273156199906580, -2.261510999192723581, 13.21476795433022211 ) ) ;
#1823 = CARTESIAN_POINT ( 'NONE',  ( 15.05486995871382483, -52.39333383871511529, 13.50000000000000178 ) ) ;
#1824 = DIRECTION ( 'NONE',  ( -1.000000000000000000, -3.387630566026860322E-15, 1.224646799147353207E-16 ) ) ;
#1825 = ORIENTED_EDGE ( 'NONE', *, *, #19313, .T. ) ;
#1826 = VERTEX_POINT ( 'NONE', #10394 ) ;
#1827 = DIRECTION ( 'NONE',  ( -0.000000000000000000, -1.000000000000000000, -0.000000000000000000 ) ) ;
#1828 = ADVANCED_FACE ( 'NONE', ( #9459 ), #21459, .T. ) ;
#1829 = LINE ( 'NONE', #6990, #21766 ) ;
#1830 = VERTEX_POINT ( 'NONE', #21570 ) ;
#1831 = AXIS2_PLACEMENT_3D ( 'NONE', #8472, #20673, #20455 ) ;
#1832 = EDGE_CURVE ( 'NONE', #10704, #5475, #3011, .T. ) ;
#1833 = AXIS2_PLACEMENT_3D ( 'NONE', #13208, #9645, #792 ) ;
#1834 = CARTESIAN_POINT ( 'NONE',  ( -1.724728116533986721, 42.36054587065083155, 51.80876104995653719 ) ) ;
#1835 = VECTOR ( 'NONE', #7797, 1000.000000000000000 ) ;
#1836 = DIRECTION ( 'NONE',  ( -0.000000000000000000, -0.000000000000000000, -1.000000000000000000 ) ) ;
#1837 = TOROIDAL_SURFACE ( 'NONE', #2913, 3.200000000000003286, 0.2999999999999999889 ) ;
#1838 = CYLINDRICAL_SURFACE ( 'NONE', #10973, 0.2500000000000002220 ) ;
#1839 = AXIS2_PLACEMENT_3D ( 'NONE', #8582, #15587, #15390 ) ;
#1840 = CARTESIAN_POINT ( 'NONE',  ( 9.141460742840918030, -33.43424481021354921, 7.321391277662001151 ) ) ;
#1841 = ORIENTED_EDGE ( 'NONE', *, *, #4561, .F. ) ;
#1842 = DIRECTION ( 'NONE',  ( 0.000000000000000000, 1.000000000000000000, 0.000000000000000000 ) ) ;
#1843 = CARTESIAN_POINT ( 'NONE',  ( 1.774728116533979438, 43.31054587065082728, 31.80876104995653719 ) ) ;
#1844 = EDGE_CURVE ( 'NONE', #6397, #19133, #15377, .T. ) ;
#1845 = CARTESIAN_POINT ( 'NONE',  ( -14.96174975910705207, 32.10873716947361345, 13.79999999999999893 ) ) ;
#1846 = FACE_OUTER_BOUND ( 'NONE', #14083, .T. ) ;
#1847 = CARTESIAN_POINT ( 'NONE',  ( -15.95292532278785913, -52.11873716947361856, 13.99999999999999822 ) ) ;
#1848 = DIRECTION ( 'NONE',  ( 0.000000000000000000, 0.000000000000000000, -1.000000000000000000 ) ) ;
#1849 = ORIENTED_EDGE ( 'NONE', *, *, #19303, .T. ) ;
#1850 = DIRECTION ( 'NONE',  ( -0.000000000000000000, -0.000000000000000000, 1.000000000000000000 ) ) ;
#1851 = CARTESIAN_POINT ( 'NONE',  ( 31.50000000000002132, -71.00000000000001421, 1.800000000000000044 ) ) ;
#1852 = ORIENTED_EDGE ( 'NONE', *, *, #14528, .T. ) ;
#1853 = VECTOR ( 'NONE', #12677, 1000.000000000000000 ) ;
#1854 = EDGE_LOOP ( 'NONE', ( #3811, #6917, #21170, #465 ) ) ;
#1855 = ORIENTED_EDGE ( 'NONE', *, *, #5162, .F. ) ;
#1856 = CARTESIAN_POINT ( 'NONE',  ( 0.000000000000000000, 39.04634676501046187, 13.79999999999999893 ) ) ;
#1857 = DIRECTION ( 'NONE',  ( 1.000000000000000000, 0.000000000000000000, -1.224646799147353207E-16 ) ) ;
#1858 = EDGE_CURVE ( 'NONE', #18170, #20955, #6345, .T. ) ;
#1859 = DIRECTION ( 'NONE',  ( -1.000000000000000000, 0.000000000000000000, 0.000000000000000000 ) ) ;
#1860 = VECTOR ( 'NONE', #2720, 1000.000000000000000 ) ;
#1861 = EDGE_CURVE ( 'NONE', #6298, #17289, #13021, .T. ) ;
#1862 = ADVANCED_FACE ( 'NONE', ( #14715 ), #6235, .T. ) ;
#1863 = VERTEX_POINT ( 'NONE', #4428 ) ;
#1864 = FACE_OUTER_BOUND ( 'NONE', #4723, .T. ) ;
#1865 = EDGE_LOOP ( 'NONE', ( #7232, #19228, #17895, #4825 ) ) ;
#1866 = DIRECTION ( 'NONE',  ( 1.000000000000000000, 0.000000000000000000, 0.000000000000000000 ) ) ;
#1867 = DIRECTION ( 'NONE',  ( 0.000000000000000000, 0.000000000000000000, 1.000000000000000000 ) ) ;
#1868 = LINE ( 'NONE', #17626, #2570 ) ;
#1869 = LINE ( 'NONE', #3668, #17343 ) ;
#1870 = EDGE_LOOP ( 'NONE', ( #9783, #17011, #19020, #1907 ) ) ;
#1871 = CARTESIAN_POINT ( 'NONE',  ( 23.02398829872513986, 2.333317872336241994, 13.47139736055077108 ) ) ;
#1872 = DIRECTION ( 'NONE',  ( -0.000000000000000000, -1.000000000000000000, 0.000000000000000000 ) ) ;
#1873 = ADVANCED_FACE ( 'NONE', ( #19875 ), #19533, .T. ) ;
#1874 = AXIS2_PLACEMENT_3D ( 'NONE', #19024, #7168, #20487 ) ;
#1875 = DIRECTION ( 'NONE',  ( 1.000000000000000000, 0.000000000000000000, 0.000000000000000000 ) ) ;
#1876 = DIRECTION ( 'NONE',  ( -1.000000000000000000, 0.000000000000000000, 0.000000000000000000 ) ) ;
#1877 = EDGE_LOOP ( 'NONE', ( #1805, #12815, #11451, #7475 ) ) ;
#1878 = CARTESIAN_POINT ( 'NONE',  ( -8.223741455913087250, 43.00645089659919051, 69.94509975324525897 ) ) ;
#1879 = DIRECTION ( 'NONE',  ( 0.000000000000000000, -1.000000000000000000, 0.000000000000000000 ) ) ;
#1880 = ORIENTED_EDGE ( 'NONE', *, *, #12667, .F. ) ;
#1881 = AXIS2_PLACEMENT_3D ( 'NONE', #10110, #3284, #17029 ) ;
#1882 = DIRECTION ( 'NONE',  ( 0.000000000000000000, 0.000000000000000000, 1.000000000000000000 ) ) ;
#1883 = CARTESIAN_POINT ( 'NONE',  ( 9.178906393579156386, 42.46645089659917716, 68.50000000000000000 ) ) ;
#1884 = ORIENTED_EDGE ( 'NONE', *, *, #16663, .F. ) ;
#1885 = EDGE_CURVE ( 'NONE', #18412, #440, #6959, .T. ) ;
#1886 = VERTEX_POINT ( 'NONE', #4216 ) ;
#1887 = EDGE_CURVE ( 'NONE', #9421, #5793, #836, .T. ) ;
#1888 = ORIENTED_EDGE ( 'NONE', *, *, #17274, .T. ) ;
#1889 = ORIENTED_EDGE ( 'NONE', *, *, #18507, .T. ) ;
#1890 = FACE_OUTER_BOUND ( 'NONE', #20607, .T. ) ;
#1891 = FACE_OUTER_BOUND ( 'NONE', #3418, .T. ) ;
#1892 = CARTESIAN_POINT ( 'NONE',  ( -1.724728116533986721, 43.26054587065083012, 35.70876104995653577 ) ) ;
#1893 = ADVANCED_FACE ( 'NONE', ( #10920 ), #6592, .F. ) ;
#1894 = CYLINDRICAL_SURFACE ( 'NONE', #16765, 0.09999999999999939493 ) ;
#1895 = EDGE_CURVE ( 'NONE', #847, #9535, #12266, .T. ) ;
#1896 = DIRECTION ( 'NONE',  ( 0.000000000000000000, 0.000000000000000000, 1.000000000000000000 ) ) ;
#1897 = VERTEX_POINT ( 'NONE', #14605 ) ;
#1898 = CARTESIAN_POINT ( 'NONE',  ( -8.134906293162368129, 43.00645089659919051, 68.06527860057354928 ) ) ;
#1899 = DIRECTION ( 'NONE',  ( -0.000000000000000000, 1.000000000000000000, -0.000000000000000000 ) ) ;
#1900 = CARTESIAN_POINT ( 'NONE',  ( -25.37540678000427263, -69.04634676501045476, 3.799999999999999822 ) ) ;
#1901 = ORIENTED_EDGE ( 'NONE', *, *, #1594, .F. ) ;
#1902 = VERTEX_POINT ( 'NONE', #17739 ) ;
#1903 = CARTESIAN_POINT ( 'NONE',  ( 31.44597781366222122, 56.94165929845684104, 68.75000000000000000 ) ) ;
#1904 = APPLICATION_PROTOCOL_DEFINITION ( 'draft international standard', 'automotive_design', 1998, #8020 ) ;
#1905 = VERTEX_POINT ( 'NONE', #12919 ) ;
#1906 = MECHANICAL_DESIGN_GEOMETRIC_PRESENTATION_REPRESENTATION (  '', ( #11918 ), #4057 ) ;
#1907 = ORIENTED_EDGE ( 'NONE', *, *, #9074, .F. ) ;
#1908 = CARTESIAN_POINT ( 'NONE',  ( 23.02398829872513986, -2.333487117377077258, 13.47150829744944467 ) ) ;
#1909 = ORIENTED_EDGE ( 'NONE', *, *, #1182, .F. ) ;
#1910 = VERTEX_POINT ( 'NONE', #16053 ) ;
#1911 = CARTESIAN_POINT ( 'NONE',  ( -1.724728116533986721, 43.26054587065083012, 45.66679706732590205 ) ) ;
#1912 = CARTESIAN_POINT ( 'NONE',  ( 1.724728116533979616, 42.31054587065082728, 47.75876104995653293 ) ) ;
#1913 = DIRECTION ( 'NONE',  ( 8.673617379884034239E-17, 0.000000000000000000, -1.000000000000000000 ) ) ;
#1914 = CARTESIAN_POINT ( 'NONE',  ( -34.70000000000000284, 85.00000000000000000, -6.019490461639519829E-15 ) ) ;
#1915 = DIRECTION ( 'NONE',  ( -0.000000000000000000, 1.000000000000000000, 0.000000000000000000 ) ) ;
#1916 = AXIS2_PLACEMENT_3D ( 'NONE', #4378, #11190, #6288 ) ;
#1917 = DIRECTION ( 'NONE',  ( -1.000000000000000000, 0.000000000000000000, 0.000000000000000000 ) ) ;
#1918 = AXIS2_PLACEMENT_3D ( 'NONE', #13554, #12288, #8529 ) ;
#1919 = ADVANCED_FACE ( 'NONE', ( #19765 ), #734, .T. ) ;
#1920 = LINE ( 'NONE', #8550, #21267 ) ;
#1921 = CARTESIAN_POINT ( 'NONE',  ( -1.724728116533986721, 43.31054587065082728, 41.71679706732590631 ) ) ;
#1922 = DIRECTION ( 'NONE',  ( -0.000000000000000000, -0.000000000000000000, -1.000000000000000000 ) ) ;
#1923 = VERTEX_POINT ( 'NONE', #12808 ) ;
#1924 = ORIENTED_EDGE ( 'NONE', *, *, #4283, .T. ) ;
#1925 = CARTESIAN_POINT ( 'NONE',  ( 29.50000000000002132, 0.000000000000000000, 0.2999999999999947153 ) ) ;
#1926 = SURFACE_STYLE_FILL_AREA ( #8766 ) ;
#1927 = LINE ( 'NONE', #10453, #7785 ) ;
#1928 = ORIENTED_EDGE ( 'NONE', *, *, #19642, .T. ) ;
#1929 = DIRECTION ( 'NONE',  ( -1.000000000000000000, 0.000000000000000000, 0.000000000000000000 ) ) ;
#1930 = EDGE_CURVE ( 'NONE', #13182, #16858, #10164, .T. ) ;
#1931 = DIRECTION ( 'NONE',  ( 1.000000000000000000, 0.000000000000000000, 0.000000000000000000 ) ) ;
#1932 = CARTESIAN_POINT ( 'NONE',  ( -27.37540678000428684, -36.74634676501047181, 42.50000000000000000 ) ) ;
#1933 = EDGE_LOOP ( 'NONE', ( #3491, #17075, #13880, #12624 ) ) ;
#1934 = LINE ( 'NONE', #5098, #4171 ) ;
#1935 = DIRECTION ( 'NONE',  ( -1.000000000000000000, 0.000000000000000000, 0.000000000000000000 ) ) ;
#1936 = EDGE_CURVE ( 'NONE', #21299, #16033, #147, .T. ) ;
#1937 = EDGE_CURVE ( 'NONE', #12578, #16703, #1507, .T. ) ;
#1938 = CYLINDRICAL_SURFACE ( 'NONE', #17448, 0.1000000000000028644 ) ;
#1939 = LINE ( 'NONE', #3742, #14627 ) ;
#1940 = CARTESIAN_POINT ( 'NONE',  ( 14.96174975910707161, -51.61873716947361856, 68.25000000000000000 ) ) ;
#1941 = ORIENTED_EDGE ( 'NONE', *, *, #15522, .T. ) ;
#1942 = DIRECTION ( 'NONE',  ( 0.000000000000000000, 0.000000000000000000, 1.000000000000000000 ) ) ;
#1943 = DIRECTION ( 'NONE',  ( 1.000000000000000000, 0.000000000000000000, 0.000000000000000000 ) ) ;
#1944 = CARTESIAN_POINT ( 'NONE',  ( -15.21174975910705207, -51.61873716947361856, 14.00000000000000000 ) ) ;
#1945 = VERTEX_POINT ( 'NONE', #13594 ) ;
#1946 = AXIS2_PLACEMENT_3D ( 'NONE', #14165, #4107, #20902 ) ;
#1947 = VERTEX_POINT ( 'NONE', #1737 ) ;
#1948 = CIRCLE ( 'NONE', #19460, 1.162443609680678280 ) ;
#1949 = ORIENTED_EDGE ( 'NONE', *, *, #12469, .T. ) ;
#1950 = CARTESIAN_POINT ( 'NONE',  ( 0.000000000000000000, -32.11873716947361856, 109.6002446535588319 ) ) ;
#1951 = DIRECTION ( 'NONE',  ( 0.000000000000000000, 0.000000000000000000, 1.000000000000000000 ) ) ;
#1952 = CARTESIAN_POINT ( 'NONE',  ( -8.638906393579159015, 44.91645089659918710, 70.88527860057354246 ) ) ;
#1953 = CARTESIAN_POINT ( 'NONE',  ( 4.127054932750481520, 32.93424481021354921, 68.50000000000000000 ) ) ;
#1954 = ADVANCED_FACE ( 'NONE', ( #21788 ), #6463, .T. ) ;
#1955 = ORIENTED_EDGE ( 'NONE', *, *, #20037, .T. ) ;
#1956 = CARTESIAN_POINT ( 'NONE',  ( 14.96174975910705918, -51.86873716947361856, 14.00000000000000000 ) ) ;
#1957 = ORIENTED_EDGE ( 'NONE', *, *, #13854, .F. ) ;
#1958 = DIRECTION ( 'NONE',  ( -0.000000000000000000, 1.000000000000000000, -0.000000000000000000 ) ) ;
#1959 = CARTESIAN_POINT ( 'NONE',  ( -9.718906393579157310, 44.91645089659918710, 70.88527860057354246 ) ) ;
#1960 = DIRECTION ( 'NONE',  ( 0.000000000000000000, -0.000000000000000000, -1.000000000000000000 ) ) ;
#1961 = VECTOR ( 'NONE', #1171, 1000.000000000000000 ) ;
#1962 = CARTESIAN_POINT ( 'NONE',  ( -29.13662752439705272, -5.299999999999999822, 7.500000000000000000 ) ) ;
#1963 = VERTEX_POINT ( 'NONE', #18397 ) ;
#1964 = CARTESIAN_POINT ( 'NONE',  ( 23.02398829872513986, 2.157133865693446229, 13.26854876702554265 ) ) ;
#1965 = DIRECTION ( 'NONE',  ( 0.000000000000000000, 0.000000000000000000, -1.000000000000000000 ) ) ;
#1966 = ADVANCED_FACE ( 'NONE', ( #6574 ), #5524, .T. ) ;
#1967 = EDGE_CURVE ( 'NONE', #14977, #8429, #3018, .T. ) ;
#1968 = DIRECTION ( 'NONE',  ( 0.000000000000000000, 0.000000000000000000, -1.000000000000000000 ) ) ;
#1969 = DIRECTION ( 'NONE',  ( -1.000000000000000000, 0.000000000000000000, 0.000000000000000000 ) ) ;
#1970 = ORIENTED_EDGE ( 'NONE', *, *, #15249, .F. ) ;
#1971 = LINE ( 'NONE', #20900, #4836 ) ;
#1972 = EDGE_CURVE ( 'NONE', #20684, #19413, #13364, .T. ) ;
#1973 = ORIENTED_EDGE ( 'NONE', *, *, #1553, .F. ) ;
#1974 = DIRECTION ( 'NONE',  ( 0.000000000000000000, -1.000000000000000000, 0.000000000000000000 ) ) ;
#1975 = VERTEX_POINT ( 'NONE', #4768 ) ;
#1976 = PRESENTATION_LAYER_ASSIGNMENT (  '', '', ( #18052 ) ) ;
#1977 = ORIENTED_EDGE ( 'NONE', *, *, #4639, .T. ) ;
#1978 = CARTESIAN_POINT ( 'NONE',  ( -6.678906393579161715, 42.46645089659918426, 61.53912392244307483 ) ) ;
#1979 = LINE ( 'NONE', #4112, #6386 ) ;
#1980 = AXIS2_PLACEMENT_3D ( 'NONE', #20327, #17069, #4881 ) ;
#1981 = ORIENTED_EDGE ( 'NONE', *, *, #9430, .T. ) ;
#1982 = VECTOR ( 'NONE', #17195, 1000.000000000000000 ) ;
#1983 = EDGE_CURVE ( 'NONE', #6378, #22039, #2291, .T. ) ;
#1984 = ORIENTED_EDGE ( 'NONE', *, *, #7152, .T. ) ;
#1985 = APPLICATION_CONTEXT ( 'automotive_design' ) ;
#1986 = VERTEX_POINT ( 'NONE', #20319 ) ;
#1987 = CARTESIAN_POINT ( 'NONE',  ( 25.37540678000427263, -63.74634676501045050, 13.50000000000000000 ) ) ;
#1988 = AXIS2_PLACEMENT_3D ( 'NONE', #9749, #14326, #10972 ) ;
#1989 = AXIS2_PLACEMENT_3D ( 'NONE', #5088, #3399, #15371 ) ;
#1990 = VECTOR ( 'NONE', #2138, 1000.000000000000000 ) ;
#1991 = CARTESIAN_POINT ( 'NONE',  ( 15.21174975910707161, 51.61873716947361856, 68.00000000000000000 ) ) ;
#1992 = CARTESIAN_POINT ( 'NONE',  ( -1.836970198721029934E-16, 71.70000000000001705, 3.200000000000000178 ) ) ;
#1993 = ADVANCED_FACE ( 'NONE', ( #16726 ), #15143, .T. ) ;
#1994 = UNCERTAINTY_MEASURE_WITH_UNIT (LENGTH_MEASURE( 1.000000000000000082E-05 ), #571, 'distance_accuracy_value', 'NONE');
#1995 = ORIENTED_EDGE ( 'NONE', *, *, #8002, .F. ) ;
#1996 = CARTESIAN_POINT ( 'NONE',  ( 29.33506712743370315, 2.703525840380863521, 0.02198462118690103911 ) ) ;
#1997 = AXIS2_PLACEMENT_3D ( 'NONE', #786, #16322, #12964 ) ;
#1998 = AXIS2_PLACEMENT_3D ( 'NONE', #16474, #18152, #2839 ) ;
#1999 = EDGE_CURVE ( 'NONE', #14884, #8585, #5888, .T. ) ;
#2000 = DIRECTION ( 'NONE',  ( 0.000000000000000000, 1.000000000000000000, 0.000000000000000000 ) ) ;
#2001 = CARTESIAN_POINT ( 'NONE',  ( 0.000000000000000000, 0.000000000000000000, 68.50000000000000000 ) ) ;
#2002 = EDGE_LOOP ( 'NONE', ( #1022, #5580, #15735, #42 ) ) ;
#2003 = DIRECTION ( 'NONE',  ( -1.000000000000000000, 0.000000000000000000, 0.000000000000000000 ) ) ;
#2004 = CARTESIAN_POINT ( 'NONE',  ( -14.66174954725422630, 51.84669727004962425, 13.50000000000000000 ) ) ;
#2005 = CIRCLE ( 'NONE', #13442, 0.2500000000000002220 ) ;
#2006 = TOROIDAL_SURFACE ( 'NONE', #14504, 0.5999999999999999778, 0.2999999999999999889 ) ;
#2007 = ORIENTED_EDGE ( 'NONE', *, *, #15662, .T. ) ;
#2008 = AXIS2_PLACEMENT_3D ( 'NONE', #19376, #15994, #16211 ) ;
#2009 = EDGE_LOOP ( 'NONE', ( #18116, #12795, #5612, #15564 ) ) ;
#2010 = LINE ( 'NONE', #5617, #18169 ) ;
#2011 = CARTESIAN_POINT ( 'NONE',  ( 0.000000000000000000, 0.000000000000000000, 82.00000000000000000 ) ) ;
#2012 = ORIENTED_EDGE ( 'NONE', *, *, #14108, .T. ) ;
#2013 = AXIS2_PLACEMENT_3D ( 'NONE', #2483, #14775, #10 ) ;
#2014 = EDGE_CURVE ( 'NONE', #11729, #6081, #20884, .T. ) ;
#2015 = CARTESIAN_POINT ( 'NONE',  ( 23.18284705826588876, -2.947275247953580202, 13.45749238763921340 ) ) ;
#2016 = ORIENTED_EDGE ( 'NONE', *, *, #7943, .T. ) ;
#2017 = ORIENTED_EDGE ( 'NONE', *, *, #17977, .F. ) ;
#2018 = DIRECTION ( 'NONE',  ( 0.000000000000000000, -1.000000000000000000, 0.000000000000000000 ) ) ;
#2019 = DIRECTION ( 'NONE',  ( 0.000000000000000000, 1.000000000000000000, 0.000000000000000000 ) ) ;
#2020 = DIRECTION ( 'NONE',  ( 0.000000000000000000, -1.000000000000000000, -0.000000000000000000 ) ) ;
#2021 = VECTOR ( 'NONE', #13684, 1000.000000000000000 ) ;
#2022 = AXIS2_PLACEMENT_3D ( 'NONE', #1213, #4596, #20044 ) ;
#2023 = CIRCLE ( 'NONE', #1304, 1.000000000000000000 ) ;
#2024 = DIRECTION ( 'NONE',  ( -7.519041366722126991E-17, 0.4461977533474358326, -0.8949343913984425525 ) ) ;
#2025 = FACE_OUTER_BOUND ( 'NONE', #152, .T. ) ;
#2026 = ADVANCED_FACE ( 'NONE', ( #1275 ), #4875, .T. ) ;
#2027 = CARTESIAN_POINT ( 'NONE',  ( -23.02398829872501906, 2.246571036181109982, 13.29719918165967840 ) ) ;
#2028 = LINE ( 'NONE', #10979, #17923 ) ;
#2029 = DIRECTION ( 'NONE',  ( 0.000000000000000000, 0.000000000000000000, 1.000000000000000000 ) ) ;
#2030 = CARTESIAN_POINT ( 'NONE',  ( 14.90249074642385807, -52.32070855895314310, 13.50000000000000355 ) ) ;
#2031 = AXIS2_PLACEMENT_3D ( 'NONE', #17973, #14830, #2886 ) ;
#2032 = CARTESIAN_POINT ( 'NONE',  ( -6.728906393579157097, 41.92645089659919933, 70.88527860057354246 ) ) ;
#2033 = ORIENTED_EDGE ( 'NONE', *, *, #19476, .T. ) ;
#2034 = EDGE_LOOP ( 'NONE', ( #7361, #18472, #3738, #4778 ) ) ;
#2035 = LINE ( 'NONE', #20957, #3148 ) ;
#2036 = LINE ( 'NONE', #10549, #9246 ) ;
#2037 = ORIENTED_EDGE ( 'NONE', *, *, #21928, .F. ) ;
#2038 = AXIS2_PLACEMENT_3D ( 'NONE', #8317, #1816, #8653 ) ;
#2039 = VECTOR ( 'NONE', #3242, 1000.000000000000000 ) ;
#2040 = CIRCLE ( 'NONE', #14538, 0.3000000000000016542 ) ;
#2041 = ADVANCED_FACE ( 'NONE', ( #11794 ), #11210, .T. ) ;
#2042 = CIRCLE ( 'NONE', #1326, 0.6999999999999992895 ) ;
#2043 = EDGE_CURVE ( 'NONE', #8135, #1711, #1571, .T. ) ;
#2044 = CIRCLE ( 'NONE', #6003, 0.04999999999999991257 ) ;
#2045 = AXIS2_PLACEMENT_3D ( 'NONE', #6921, #20775, #1857 ) ;
#2046 = DIRECTION ( 'NONE',  ( -0.000000000000000000, -0.000000000000000000, -1.000000000000000000 ) ) ;
#2047 = DIRECTION ( 'NONE',  ( 0.000000000000000000, 0.000000000000000000, 1.000000000000000000 ) ) ;
#2048 = ORIENTED_EDGE ( 'NONE', *, *, #2373, .F. ) ;
#2049 = DIRECTION ( 'NONE',  ( 0.000000000000000000, 0.000000000000000000, 1.000000000000000000 ) ) ;
#2050 = CYLINDRICAL_SURFACE ( 'NONE', #15329, 0.1000000000000028644 ) ;
#2051 = LINE ( 'NONE', #7327, #2553 ) ;
#2052 = DIRECTION ( 'NONE',  ( -0.000000000000000000, -0.000000000000000000, -1.000000000000000000 ) ) ;
#2053 = CARTESIAN_POINT ( 'NONE',  ( -14.66174975910705136, 51.76873716947361714, 13.50000000000000000 ) ) ;
#2054 = AXIS2_PLACEMENT_3D ( 'NONE', #751, #11158, #12602 ) ;
#2055 = AXIS2_PLACEMENT_3D ( 'NONE', #17648, #2552, #3918 ) ;
#2056 = AXIS2_PLACEMENT_3D ( 'NONE', #20807, #12160, #15846 ) ;
#2057 = DIRECTION ( 'NONE',  ( -1.000000000000000000, 0.000000000000000000, 0.000000000000000000 ) ) ;
#2058 = ORIENTED_EDGE ( 'NONE', *, *, #14084, .F. ) ;
#2059 = DIRECTION ( 'NONE',  ( 0.000000000000000000, -1.000000000000000000, 0.000000000000000000 ) ) ;
#2060 = CARTESIAN_POINT ( 'NONE',  ( 1.774728116533979438, 43.31054587065082728, 35.80876104995653009 ) ) ;
#2061 = AXIS2_PLACEMENT_3D ( 'NONE', #7276, #17554, #19124 ) ;
#2062 = CARTESIAN_POINT ( 'NONE',  ( 1.724728116533979838, 43.31054587065082728, 37.66679706732590915 ) ) ;
#2063 = EDGE_CURVE ( 'NONE', #9364, #97, #14073, .T. ) ;
#2064 = ORIENTED_EDGE ( 'NONE', *, *, #12333, .F. ) ;
#2065 = ORIENTED_EDGE ( 'NONE', *, *, #12737, .T. ) ;
#2066 = CIRCLE ( 'NONE', #13848, 0.04999999999999991257 ) ;
#2067 = ORIENTED_EDGE ( 'NONE', *, *, #6555, .F. ) ;
#2068 = CARTESIAN_POINT ( 'NONE',  ( 33.49999999999998579, 84.70000000000001705, 78.50000000000000000 ) ) ;
#2069 = DIRECTION ( 'NONE',  ( 0.000000000000000000, -0.000000000000000000, 1.000000000000000000 ) ) ;
#2070 = AXIS2_PLACEMENT_3D ( 'NONE', #14269, #8918, #7577 ) ;
#2071 = CARTESIAN_POINT ( 'NONE',  ( -29.50000000000002132, 0.000000000000000000, -150.0833101980363722 ) ) ;
#2072 = CYLINDRICAL_SURFACE ( 'NONE', #13846, 4.193574995607837863 ) ;
#2073 = ADVANCED_FACE ( 'NONE', ( #18739 ), #12989, .T. ) ;
#2074 = ORIENTED_EDGE ( 'NONE', *, *, #5013, .T. ) ;
#2075 = DIRECTION ( 'NONE',  ( 0.000000000000000000, 1.000000000000000000, 0.000000000000000000 ) ) ;
#2076 = CIRCLE ( 'NONE', #16717, 6.499999999999999112 ) ;
#2077 = VECTOR ( 'NONE', #16297, 1000.000000000000000 ) ;
#2078 = VERTEX_POINT ( 'NONE', #15385 ) ;
#2079 = DIRECTION ( 'NONE',  ( 1.000000000000000000, 0.000000000000000000, 0.000000000000000000 ) ) ;
#2080 = CARTESIAN_POINT ( 'NONE',  ( 15.95292532278785913, -52.39333383871510108, 13.79999999999999893 ) ) ;
#2081 = CIRCLE ( 'NONE', #14232, 1.750000000000001554 ) ;
#2082 = CARTESIAN_POINT ( 'NONE',  ( 1.724728116533979838, 42.36054587065083155, 37.66679706732590915 ) ) ;
#2083 = AXIS2_PLACEMENT_3D ( 'NONE', #12956, #9289, #773 ) ;
#2084 = CARTESIAN_POINT ( 'NONE',  ( 0.000000000000000000, 42.31054587065082728, 29.71679706732590631 ) ) ;
#2085 = VERTEX_POINT ( 'NONE', #18298 ) ;
#2086 = CARTESIAN_POINT ( 'NONE',  ( 1.774728116533973665, 43.26054587065083012, 16.00000000000000000 ) ) ;
#2087 = VECTOR ( 'NONE', #14409, 1000.000000000000000 ) ;
#2088 = CARTESIAN_POINT ( 'NONE',  ( 8.641460742840918030, -33.43424481021354921, 68.00000000000000000 ) ) ;
#2089 = LINE ( 'NONE', #3674, #10507 ) ;
#2090 = DIRECTION ( 'NONE',  ( 1.000000000000000000, 0.000000000000000000, 0.000000000000000000 ) ) ;
#2091 = EDGE_LOOP ( 'NONE', ( #18512, #12254, #12155, #5768 ) ) ;
#2092 = CARTESIAN_POINT ( 'NONE',  ( -1.824728116533986810, 42.36054587065083155, 45.66679706732590205 ) ) ;
#2093 = EDGE_CURVE ( 'NONE', #3329, #19467, #5664, .T. ) ;
#2094 = ORIENTED_EDGE ( 'NONE', *, *, #4035, .F. ) ;
#2095 = FACE_OUTER_BOUND ( 'NONE', #10503, .T. ) ;
#2096 = DIRECTION ( 'NONE',  ( 1.000000000000000000, 2.832483164223420229E-16, 0.000000000000000000 ) ) ;
#2097 = TOROIDAL_SURFACE ( 'NONE', #13963, 0.05000000000000000278, 0.05000000000000000278 ) ;
#2098 = ORIENTED_EDGE ( 'NONE', *, *, #3725, .F. ) ;
#2099 = VERTEX_POINT ( 'NONE', #13914 ) ;
#2100 = FACE_OUTER_BOUND ( 'NONE', #12467, .T. ) ;
#2101 = LINE ( 'NONE', #20908, #4931 ) ;
#2102 = CIRCLE ( 'NONE', #16762, 0.5999999999999999778 ) ;
#2103 = VERTEX_POINT ( 'NONE', #3975 ) ;
#2104 = AXIS2_PLACEMENT_3D ( 'NONE', #11045, #19891, #17753 ) ;
#2105 = ADVANCED_FACE ( 'NONE', ( #1846 ), #17270, .F. ) ;
#2106 = EDGE_CURVE ( 'NONE', #8651, #6754, #5543, .T. ) ;
#2107 = EDGE_CURVE ( 'NONE', #8250, #16620, #1210, .T. ) ;
#2108 = VERTEX_POINT ( 'NONE', #262 ) ;
#2109 = ORIENTED_EDGE ( 'NONE', *, *, #20482, .T. ) ;
#2110 = DIRECTION ( 'NONE',  ( -0.000000000000000000, -0.000000000000000000, -1.000000000000000000 ) ) ;
#2111 = DIRECTION ( 'NONE',  ( 0.000000000000000000, -1.000000000000000000, 0.000000000000000000 ) ) ;
#2112 = CARTESIAN_POINT ( 'NONE',  ( -8.641460742840918030, -32.93424481021354921, 7.321391277662001151 ) ) ;
#2113 = CARTESIAN_POINT ( 'NONE',  ( 29.13662752439705272, -5.299999999999999822, 7.200000000000000178 ) ) ;
#2114 = AXIS2_PLACEMENT_3D ( 'NONE', #5387, #12612, #13967 ) ;
#2115 = CYLINDRICAL_SURFACE ( 'NONE', #5635, 0.5000000000000000000 ) ;
#2116 = ORIENTED_EDGE ( 'NONE', *, *, #16280, .F. ) ;
#2117 = CARTESIAN_POINT ( 'NONE',  ( -18.05178606074127501, 38.87061083372239523, 13.49999999999999822 ) ) ;
#2118 = EDGE_CURVE ( 'NONE', #21063, #10017, #19447, .T. ) ;
#2119 = CARTESIAN_POINT ( 'NONE',  ( -1.724728116533986721, 43.26054587065083012, 49.71679706732589921 ) ) ;
#2120 = LINE ( 'NONE', #8955, #432 ) ;
#2121 = ORIENTED_EDGE ( 'NONE', *, *, #16881, .F. ) ;
#2122 = CARTESIAN_POINT ( 'NONE',  ( -29.69597781366221412, 27.99124249474150972, 70.25000000000000000 ) ) ;
#2123 = VECTOR ( 'NONE', #7005, 1000.000000000000000 ) ;
#2124 = EDGE_LOOP ( 'NONE', ( #9690, #21999, #1691, #21101 ) ) ;
#2125 = FACE_OUTER_BOUND ( 'NONE', #19633, .T. ) ;
#2126 = APPLICATION_PROTOCOL_DEFINITION ( 'draft international standard', 'automotive_design', 1998, #5452 ) ;
#2127 = EDGE_CURVE ( 'NONE', #5807, #3080, #9811, .T. ) ;
#2128 = AXIS2_PLACEMENT_3D ( 'NONE', #21365, #11161, #16291 ) ;
#2129 = ORIENTED_EDGE ( 'NONE', *, *, #8000, .F. ) ;
#2130 = AXIS2_PLACEMENT_3D ( 'NONE', #10660, #354, #15788 ) ;
#2131 = EDGE_CURVE ( 'NONE', #9554, #10005, #10718, .T. ) ;
#2132 = ORIENTED_EDGE ( 'NONE', *, *, #12800, .F. ) ;
#2133 = ADVANCED_FACE ( 'NONE', ( #13795 ), #5734, .T. ) ;
#2134 = CARTESIAN_POINT ( 'NONE',  ( 32.20000000000001705, 71.00000000000001421, 1.500000000000000000 ) ) ;
#2135 = EDGE_LOOP ( 'NONE', ( #16925, #18666, #12516, #12086 ) ) ;
#2136 = VERTEX_POINT ( 'NONE', #2274 ) ;
#2137 = LINE ( 'NONE', #555, #7712 ) ;
#2138 = DIRECTION ( 'NONE',  ( -2.832483164223434527E-16, 1.000000000000000000, 0.000000000000000000 ) ) ;
#2139 = CARTESIAN_POINT ( 'NONE',  ( 14.66174975910705847, -42.11054587065083155, 13.50000000000000000 ) ) ;
#2140 = DIRECTION ( 'NONE',  ( -1.000000000000000000, 0.000000000000000000, 0.000000000000000000 ) ) ;
#2141 = AXIS2_PLACEMENT_3D ( 'NONE', #5791, #14370, #21222 ) ;
#2142 = EDGE_CURVE ( 'NONE', #2941, #17988, #12323, .T. ) ;
#2143 = AXIS2_PLACEMENT_3D ( 'NONE', #19320, #84, #13824 ) ;
#2144 = CARTESIAN_POINT ( 'NONE',  ( -23.02398829872513986, 2.388718329487966585, 13.39778868030486514 ) ) ;
#2145 = CARTESIAN_POINT ( 'NONE',  ( 27.37540678000427619, 7.754037881813018962E-15, 42.50000000000000000 ) ) ;
#2146 = CARTESIAN_POINT ( 'NONE',  ( 23.32398829872514412, -3.528912754968634768, 13.50000000000000000 ) ) ;
#2147 = FACE_OUTER_BOUND ( 'NONE', #2934, .T. ) ;
#2148 = EDGE_CURVE ( 'NONE', #7257, #15319, #6807, .T. ) ;
#2149 = CARTESIAN_POINT ( 'NONE',  ( 30.79999999999999716, 69.70000000000000284, 4.029087969194791265E-15 ) ) ;
#2150 = ORIENTED_EDGE ( 'NONE', *, *, #1136, .F. ) ;
#2151 = ORIENTED_EDGE ( 'NONE', *, *, #6149, .F. ) ;
#2152 = CARTESIAN_POINT ( 'NONE',  ( 27.77120804565220169, -2.094189496455408861, 1.500000000000000666 ) ) ;
#2153 = SHAPE_REPRESENTATION_RELATIONSHIP ( 'NONE' , 'NONE' ,  #9407, #7548 ) ;
#2154 = CARTESIAN_POINT ( 'NONE',  ( -14.71174975910705029, 51.61873716947361856, 14.00000000000000000 ) ) ;
#2155 = ORIENTED_EDGE ( 'NONE', *, *, #20663, .T. ) ;
#2156 = ORIENTED_EDGE ( 'NONE', *, *, #100, .T. ) ;
#2157 = EDGE_CURVE ( 'NONE', #1357, #13818, #20974, .T. ) ;
#2158 = AXIS2_PLACEMENT_3D ( 'NONE', #17896, #9406, #19700 ) ;
#2159 = CIRCLE ( 'NONE', #8244, 1.000000000000000888 ) ;
#2160 = DIRECTION ( 'NONE',  ( -1.000000000000000000, 0.000000000000000000, 0.000000000000000000 ) ) ;
#2161 = CARTESIAN_POINT ( 'NONE',  ( 32.50000000000002132, -71.00000000000001421, 1.800000000000000044 ) ) ;
#2162 = ORIENTED_EDGE ( 'NONE', *, *, #8500, .F. ) ;
#2163 = DIRECTION ( 'NONE',  ( 1.000000000000000000, 0.000000000000000000, 0.000000000000000000 ) ) ;
#2164 = PLANE ( 'NONE',  #5351 ) ;
#2165 = FACE_OUTER_BOUND ( 'NONE', #18868, .T. ) ;
#2166 = DIRECTION ( 'NONE',  ( 1.000000000000000000, 0.000000000000000000, 0.000000000000000000 ) ) ;
#2167 = LINE ( 'NONE', #4182, #7945 ) ;
#2168 = CARTESIAN_POINT ( 'NONE',  ( -33.50000000000001421, 85.00000000000000000, 80.00000000000000000 ) ) ;
#2169 = CARTESIAN_POINT ( 'NONE',  ( -3.127054932750481964, 32.61873716947361856, 68.50000000000000000 ) ) ;
#2170 = EDGE_CURVE ( 'NONE', #7987, #416, #8929, .T. ) ;
#2171 = DIRECTION ( 'NONE',  ( 0.000000000000000000, 0.000000000000000000, 1.000000000000000000 ) ) ;
#2172 = CIRCLE ( 'NONE', #2529, 0.2500000000000002220 ) ;
#2173 = DIRECTION ( 'NONE',  ( 0.000000000000000000, 0.000000000000000000, 1.000000000000000000 ) ) ;
#2174 = ADVANCED_FACE ( 'NONE', ( #10685 ), #588, .F. ) ;
#2175 = CARTESIAN_POINT ( 'NONE',  ( 1.824728116533979705, 42.36054587065083155, 37.66679706732590915 ) ) ;
#2176 = ADVANCED_FACE ( 'NONE', ( #20653 ), #8896, .T. ) ;
#2177 = EDGE_LOOP ( 'NONE', ( #13663, #12113, #12764, #7426 ) ) ;
#2178 = ORIENTED_EDGE ( 'NONE', *, *, #2506, .F. ) ;
#2179 = VERTEX_POINT ( 'NONE', #15583 ) ;
#2180 = LINE ( 'NONE', #19411, #8851 ) ;
#2181 = CARTESIAN_POINT ( 'NONE',  ( -23.02398829872513986, 7.027230193580998154E-15, 42.50000000000000000 ) ) ;
#2182 = FACE_OUTER_BOUND ( 'NONE', #14690, .T. ) ;
#2183 = ORIENTED_EDGE ( 'NONE', *, *, #4758, .F. ) ;
#2184 = ADVANCED_BREP_SHAPE_REPRESENTATION ( '', ( #5668, #17493 ), #14991 ) ;
#2185 = DIRECTION ( 'NONE',  ( 0.000000000000000000, 0.000000000000000000, -1.000000000000000000 ) ) ;
#2186 = AXIS2_PLACEMENT_3D ( 'NONE', #4661, #11471, #2636 ) ;
#2187 = AXIS2_PLACEMENT_3D ( 'NONE', #9890, #18039, #18377 ) ;
#2188 = ORIENTED_EDGE ( 'NONE', *, *, #9154, .F. ) ;
#2189 = DIRECTION ( 'NONE',  ( -0.000000000000000000, 1.000000000000000000, -0.000000000000000000 ) ) ;
#2190 = CARTESIAN_POINT ( 'NONE',  ( 15.95292532278785913, -50.11873716947361856, 68.00000000000000000 ) ) ;
#2191 = ORIENTED_EDGE ( 'NONE', *, *, #21928, .T. ) ;
#2192 = DIRECTION ( 'NONE',  ( 0.000000000000000000, 0.000000000000000000, -1.000000000000000000 ) ) ;
#2193 = AXIS2_PLACEMENT_3D ( 'NONE', #12575, #5565, #20887 ) ;
#2194 = CYLINDRICAL_SURFACE ( 'NONE', #1362, 0.2999999999999947153 ) ;
#2195 = DIRECTION ( 'NONE',  ( 0.000000000000000000, 0.000000000000000000, -1.000000000000000000 ) ) ;
#2196 = CARTESIAN_POINT ( 'NONE',  ( 25.37540678000427263, -67.24634676501045760, 7.799999999999999822 ) ) ;
#2197 = ORIENTED_EDGE ( 'NONE', *, *, #16341, .F. ) ;
#2198 = DIRECTION ( 'NONE',  ( -0.000000000000000000, 0.000000000000000000, -1.000000000000000000 ) ) ;
#2199 = CARTESIAN_POINT ( 'NONE',  ( -8.641460742840918030, -32.93424481021354921, 68.50000000000000000 ) ) ;
#2200 = FACE_OUTER_BOUND ( 'NONE', #12642, .T. ) ;
#2201 = DIRECTION ( 'NONE',  ( 0.000000000000000000, 0.000000000000000000, 1.000000000000000000 ) ) ;
#2202 = ORIENTED_EDGE ( 'NONE', *, *, #21718, .F. ) ;
#2203 = FACE_OUTER_BOUND ( 'NONE', #16007, .T. ) ;
#2204 = AXIS2_PLACEMENT_3D ( 'NONE', #19026, #4124, #10944 ) ;
#2205 = EDGE_CURVE ( 'NONE', #13894, #10046, #9649, .T. ) ;
#2206 = ORIENTED_EDGE ( 'NONE', *, *, #8421, .T. ) ;
#2207 = LINE ( 'NONE', #21019, #6625 ) ;
#2208 = AXIS2_PLACEMENT_3D ( 'NONE', #7099, #18607, #6653 ) ;
#2209 = DIRECTION ( 'NONE',  ( 1.000000000000000000, 0.000000000000000000, 0.000000000000000000 ) ) ;
#2210 = EDGE_CURVE ( 'NONE', #3697, #3514, #1939, .T. ) ;
#2211 = VERTEX_POINT ( 'NONE', #17380 ) ;
#2212 = VERTEX_POINT ( 'NONE', #7225 ) ;
#2213 = DIRECTION ( 'NONE',  ( 0.000000000000000000, 0.000000000000000000, -1.000000000000000000 ) ) ;
#2214 = CARTESIAN_POINT ( 'NONE',  ( -33.80000000000000426, -85.00000000000000000, 1.800000000000000266 ) ) ;
#2215 = EDGE_LOOP ( 'NONE', ( #591, #18324, #11991, #10747 ) ) ;
#2216 = ORIENTED_EDGE ( 'NONE', *, *, #20848, .F. ) ;
#2217 = AXIS2_PLACEMENT_3D ( 'NONE', #5414, #5638, #10540 ) ;
#2218 = DIRECTION ( 'NONE',  ( -0.000000000000000000, 0.000000000000000000, 1.000000000000000000 ) ) ;
#2219 = CARTESIAN_POINT ( 'NONE',  ( -1.824728116533986810, 42.36054587065083155, 47.75876104995653293 ) ) ;
#2220 = AXIS2_PLACEMENT_3D ( 'NONE', #1422, #20020, #4687 ) ;
#2221 = CARTESIAN_POINT ( 'NONE',  ( -3.627054932750481964, -33.43424481021354921, 68.00000000000000000 ) ) ;
#2222 = DIRECTION ( 'NONE',  ( 0.000000000000000000, 1.000000000000000000, -0.000000000000000000 ) ) ;
#2223 = CARTESIAN_POINT ( 'NONE',  ( 1.724728116533979838, 42.31054587065082728, 29.66679706732590560 ) ) ;
#2224 = ORIENTED_EDGE ( 'NONE', *, *, #14838, .T. ) ;
#2225 = DIRECTION ( 'NONE',  ( 1.000000000000000000, 0.000000000000000000, 0.000000000000000000 ) ) ;
#2226 = ADVANCED_FACE ( 'NONE', ( #3861 ), #1053, .T. ) ;
#2227 = PLANE ( 'NONE',  #6244 ) ;
#2228 = ADVANCED_FACE ( 'NONE', ( #21098 ), #8570, .F. ) ;
#2229 = FACE_BOUND ( 'NONE', #21263, .T. ) ;
#2230 = VERTEX_POINT ( 'NONE', #703 ) ;
#2231 = CIRCLE ( 'NONE', #20108, 6.499999999999999112 ) ;
#2232 = DIRECTION ( 'NONE',  ( 1.000000000000000000, 0.000000000000000000, -2.388292521039847891E-16 ) ) ;
#2233 = ORIENTED_EDGE ( 'NONE', *, *, #11870, .T. ) ;
#2234 = AXIS2_PLACEMENT_3D ( 'NONE', #2307, #15941, #626 ) ;
#2235 = EDGE_LOOP ( 'NONE', ( #710, #15792, #1731, #16469 ) ) ;
#2236 = DIRECTION ( 'NONE',  ( 1.000000000000000000, 0.000000000000000000, 0.000000000000000000 ) ) ;
#2237 = APPLICATION_PROTOCOL_DEFINITION ( 'draft international standard', 'automotive_design', 1998, #13849 ) ;
#2238 = VERTEX_POINT ( 'NONE', #4400 ) ;
#2239 = ORIENTED_EDGE ( 'NONE', *, *, #13708, .T. ) ;
#2240 = EDGE_CURVE ( 'NONE', #6576, #10531, #21441, .T. ) ;
#2241 = CARTESIAN_POINT ( 'NONE',  ( 23.02398829872478814, -2.211005313988728016, 13.25071573983089834 ) ) ;
#2242 = VERTEX_POINT ( 'NONE', #21205 ) ;
#2243 = VERTEX_POINT ( 'NONE', #19501 ) ;
#2244 = FACE_OUTER_BOUND ( 'NONE', #3294, .T. ) ;
#2245 = DIRECTION ( 'NONE',  ( 0.000000000000000000, 0.000000000000000000, -1.000000000000000000 ) ) ;
#2246 = DIRECTION ( 'NONE',  ( -6.123233995736764803E-17, 0.000000000000000000, 1.000000000000000000 ) ) ;
#2247 = CARTESIAN_POINT ( 'NONE',  ( 25.37540678000427263, -63.74634676501045050, 7.200000000000000178 ) ) ;
#2248 = CARTESIAN_POINT ( 'NONE',  ( -14.96174975910705207, 51.61873716947361856, 68.00000000000000000 ) ) ;
#2249 = EDGE_CURVE ( 'NONE', #6000, #1830, #12480, .T. ) ;
#2250 = EDGE_CURVE ( 'NONE', #10557, #21684, #15350, .T. ) ;
#2251 = CARTESIAN_POINT ( 'NONE',  ( 28.79994065384636315, 6.566898051583388352, 13.40260211333369256 ) ) ;
#2252 = EDGE_CURVE ( 'NONE', #17256, #21160, #15598, .T. ) ;
#2253 = DIRECTION ( 'NONE',  ( 0.000000000000000000, 0.000000000000000000, 1.000000000000000000 ) ) ;
#2254 = CARTESIAN_POINT ( 'NONE',  ( 0.000000000000000000, 42.31054587065082728, 53.71679706732590631 ) ) ;
#2255 = FACE_OUTER_BOUND ( 'NONE', #15549, .T. ) ;
#2256 = EDGE_CURVE ( 'NONE', #17559, #19811, #777, .T. ) ;
#2257 = LINE ( 'NONE', #10544, #16014 ) ;
#2258 = VERTEX_POINT ( 'NONE', #5623 ) ;
#2259 = ORIENTED_EDGE ( 'NONE', *, *, #22111, .T. ) ;
#2260 = CARTESIAN_POINT ( 'NONE',  ( 0.000000000000000000, -5.299999999999999822, 7.200000000000000178 ) ) ;
#2261 = CARTESIAN_POINT ( 'NONE',  ( -9.178906393579158163, 42.46645089659918426, 68.06527860057354928 ) ) ;
#2262 = ORIENTED_EDGE ( 'NONE', *, *, #4621, .T. ) ;
#2263 = EDGE_LOOP ( 'NONE', ( #18702, #12930, #6688, #1174 ) ) ;
#2264 = EDGE_LOOP ( 'NONE', ( #1021, #18937, #21411, #2525 ) ) ;
#2265 = ADVANCED_FACE ( 'NONE', ( #5400 ), #16115, .F. ) ;
#2266 = CARTESIAN_POINT ( 'NONE',  ( -25.37540678000427263, -63.74634676501045050, 3.799999999999999822 ) ) ;
#2267 =( BOUNDED_SURFACE ( )  B_SPLINE_SURFACE ( 3, 2, ( 
 ( #21869, #1585, #11878 ),
 ( #1369, #8321, #8420 ),
 ( #15239, #13568, #8217 ),
 ( #13670, #18829, #6551 ),
 ( #20174, #4842, #11653 ),
 ( #12300, #681, #12424 ),
 ( #14221, #10539, #15677 ),
 ( #454, #2144, #5636 ),
 ( #10866, #17249, #19274 ),
 ( #17680, #2027, #10657 ),
 ( #5413, #10441, #14329 ),
 ( #15556, #20738, #16002 ) ),
 .UNSPECIFIED., .F., .F., .F. ) 
 B_SPLINE_SURFACE_WITH_KNOTS ( ( 4, 2, 2, 2, 2, 4 ),
 ( 3, 3 ),
 ( 0.0006083281319963878804, 0.001004469391314931435, 0.001400610650633475097, 0.001796751909952018760, 0.001994822539611290808, 0.002192893169270562423 ),
 ( 0.000000000000000000, 1.000000000000000000 ),
 .UNSPECIFIED. ) 
 GEOMETRIC_REPRESENTATION_ITEM ( )  RATIONAL_B_SPLINE_SURFACE ( (
 ( 1.000000000000000000, 0.7071067811865475727, 1.000000000000000000),
 ( 1.000000000000000000, 0.7419362082869511710, 1.000000000000000000),
 ( 1.000000000000000000, 0.7734000586050161496, 1.000000000000000000),
 ( 1.000000000000000000, 0.8313348272087629498, 1.000000000000000000),
 ( 1.000000000000000000, 0.8578042680912283391, 1.000000000000000000),
 ( 1.000000000000000000, 0.9064979099737326962, 1.000000000000000000),
 ( 1.000000000000000000, 0.9284078965777999848, 1.000000000000000000),
 ( 1.000000000000000000, 0.9565959158316897915, 1.000000000000000000),
 ( 1.000000000000000000, 0.9652268734598790090, 1.000000000000000000),
 ( 1.000000000000000000, 0.9789818400845240465, 1.000000000000000000),
 ( 1.000000000000000000, 0.9843224408025279537, 1.000000000000000000),
 ( 1.000000000000000000, 0.9842566880020492404, 1.000000000000000000) ) ) 
 REPRESENTATION_ITEM ( '' )  SURFACE ( )  );
#2268 = CYLINDRICAL_SURFACE ( 'NONE', #13076, 0.2999999999999999334 ) ;
#2269 = VERTEX_POINT ( 'NONE', #17575 ) ;
#2270 = DIRECTION ( 'NONE',  ( 0.000000000000000000, 0.000000000000000000, 1.000000000000000000 ) ) ;
#2271 = CARTESIAN_POINT ( 'NONE',  ( 23.11743451022278251, 2.646042693280193703, 13.40127653599240531 ) ) ;
#2272 = CARTESIAN_POINT ( 'NONE',  ( 15.21174975910707161, -42.31054587065082728, 68.50000000000000000 ) ) ;
#2273 = EDGE_CURVE ( 'NONE', #4102, #17715, #4043, .T. ) ;
#2274 = CARTESIAN_POINT ( 'NONE',  ( -15.21174975910705207, 41.81054587065082728, 68.50000000000000000 ) ) ;
#2275 = DIRECTION ( 'NONE',  ( 0.000000000000000000, 0.000000000000000000, 1.000000000000000000 ) ) ;
#2276 = CARTESIAN_POINT ( 'NONE',  ( -29.13662752439705272, -5.000000000000000000, 3.799999999999999822 ) ) ;
#2277 = EDGE_CURVE ( 'NONE', #5258, #6865, #17925, .T. ) ;
#2278 = AXIS2_PLACEMENT_3D ( 'NONE', #12252, #625, #12358 ) ;
#2279 = DIRECTION ( 'NONE',  ( 1.000000000000000000, 0.000000000000000000, 0.000000000000000000 ) ) ;
#2280 = CARTESIAN_POINT ( 'NONE',  ( -29.13662752439705272, -5.000000000000000000, 7.500000000000000000 ) ) ;
#2281 = CARTESIAN_POINT ( 'NONE',  ( -29.69597781366221767, 58.94165929845684815, 70.25000000000000000 ) ) ;
#2282 = ORIENTED_EDGE ( 'NONE', *, *, #7746, .F. ) ;
#2283 = ORIENTED_EDGE ( 'NONE', *, *, #8754, .T. ) ;
#2284 = ORIENTED_EDGE ( 'NONE', *, *, #20612, .T. ) ;
#2285 = CARTESIAN_POINT ( 'NONE',  ( 27.69541703706358504, -2.215671135867736119, 0.03255948639529124972 ) ) ;
#2286 = DIRECTION ( 'NONE',  ( -1.000000000000000000, 0.000000000000000000, 0.000000000000000000 ) ) ;
#2287 = ORIENTED_EDGE ( 'NONE', *, *, #7882, .F. ) ;
#2288 = CIRCLE ( 'NONE', #14788, 0.5000000000000004441 ) ;
#2289 = DIRECTION ( 'NONE',  ( 0.000000000000000000, 0.000000000000000000, 1.000000000000000000 ) ) ;
#2290 = FACE_OUTER_BOUND ( 'NONE', #1311, .T. ) ;
#2291 = CIRCLE ( 'NONE', #2645, 0.2500000000000002220 ) ;
#2292 = EDGE_LOOP ( 'NONE', ( #19235, #14828, #13607, #6975, #2767, #19204, #20216, #13606, #10636, #16852, #6582, #4263, #3988, #4387, #9907, #16735, #7318, #3557, #13548, #20008, #19285 ) ) ;
#2293 = DIRECTION ( 'NONE',  ( -1.000000000000000000, 0.000000000000000000, 0.000000000000000000 ) ) ;
#2294 = CARTESIAN_POINT ( 'NONE',  ( -1.774728116533986766, 43.26054587065083012, 49.66679706732590915 ) ) ;
#2295 = EDGE_CURVE ( 'NONE', #14227, #852, #5512, .T. ) ;
#2296 = VERTEX_POINT ( 'NONE', #7188 ) ;
#2297 = DIRECTION ( 'NONE',  ( -0.2309407893632113573, 0.9729678061520313781, 0.000000000000000000 ) ) ;
#2298 = EDGE_CURVE ( 'NONE', #1170, #8695, #13984, .T. ) ;
#2299 = DIRECTION ( 'NONE',  ( 0.000000000000000000, 0.000000000000000000, 1.000000000000000000 ) ) ;
#2300 = B_SPLINE_CURVE_WITH_KNOTS ( 'NONE', 3,
 ( #17616, #384, #3755, #2285, #7457, #7562 ),
 .UNSPECIFIED., .F., .F.,
 ( 4, 2, 4 ),
 ( 3.442662021193151749E-18, 0.0002343895398574032151, 0.0004687790797148030150 ),
 .UNSPECIFIED. ) ;
#2301 = CYLINDRICAL_SURFACE ( 'NONE', #13994, 0.2999999999999999334 ) ;
#2302 = CARTESIAN_POINT ( 'NONE',  ( -1.824728116533986810, 43.31054587065082728, 29.76679706732590702 ) ) ;
#2303 = EDGE_LOOP ( 'NONE', ( #819, #3702, #11434, #5971 ) ) ;
#2304 = CARTESIAN_POINT ( 'NONE',  ( -1.824728116533986810, 43.26054587065083012, 31.80876104995653719 ) ) ;
#2305 = CYLINDRICAL_SURFACE ( 'NONE', #3890, 0.04999999999999991257 ) ;
#2306 = CARTESIAN_POINT ( 'NONE',  ( -26.37540678000427619, -10.94079601157914716, 42.50000000000000000 ) ) ;
#2307 = CARTESIAN_POINT ( 'NONE',  ( 27.67540678000428400, -36.74634676501047181, 13.79999999999999893 ) ) ;
#2308 = ORIENTED_EDGE ( 'NONE', *, *, #18668, .F. ) ;
#2309 = DIRECTION ( 'NONE',  ( 1.000000000000000000, 0.000000000000000000, 6.123233995736764803E-17 ) ) ;
#2310 = AXIS2_PLACEMENT_3D ( 'NONE', #18950, #6985, #2029 ) ;
#2311 = EDGE_CURVE ( 'NONE', #17419, #5726, #13288, .T. ) ;
#2312 = EDGE_LOOP ( 'NONE', ( #21198, #12646, #9893, #7341 ) ) ;
#2313 = DIRECTION ( 'NONE',  ( 0.000000000000000000, 1.000000000000000000, 0.000000000000000000 ) ) ;
#2314 = LINE ( 'NONE', #7157, #14880 ) ;
#2315 = ORIENTED_EDGE ( 'NONE', *, *, #1416, .T. ) ;
#2316 = ORIENTED_EDGE ( 'NONE', *, *, #17890, .F. ) ;
#2317 = DIRECTION ( 'NONE',  ( -0.000000000000000000, 1.000000000000000000, 0.000000000000000000 ) ) ;
#2318 = FACE_OUTER_BOUND ( 'NONE', #11703, .T. ) ;
#2319 = VERTEX_POINT ( 'NONE', #17669 ) ;
#2320 = VERTEX_POINT ( 'NONE', #2134 ) ;
#2321 = AXIS2_PLACEMENT_3D ( 'NONE', #7261, #5053, #19333 ) ;
#2322 = CIRCLE ( 'NONE', #14820, 0.5999999999999998668 ) ;
#2323 = ADVANCED_FACE ( 'NONE', ( #671 ), #17220, .T. ) ;
#2324 = VERTEX_POINT ( 'NONE', #5294 ) ;
#2325 = DIRECTION ( 'NONE',  ( 1.000000000000000000, 0.000000000000000000, 0.000000000000000000 ) ) ;
#2326 = ADVANCED_FACE ( 'NONE', ( #782 ), #4143, .F. ) ;
#2327 = DIRECTION ( 'NONE',  ( -0.000000000000000000, -1.000000000000000000, -0.000000000000000000 ) ) ;
#2328 = DIRECTION ( 'NONE',  ( 2.107255972849994642E-16, -0.000000000000000000, 1.000000000000000000 ) ) ;
#2329 = CARTESIAN_POINT ( 'NONE',  ( 1.724728116533979838, 43.31054587065082728, 33.66679706732590915 ) ) ;
#2330 = ORIENTED_EDGE ( 'NONE', *, *, #7422, .T. ) ;
#2331 = CARTESIAN_POINT ( 'NONE',  ( -14.96174975910705207, 41.81054587065082728, 13.75000000000000000 ) ) ;
#2332 = AXIS2_PLACEMENT_3D ( 'NONE', #8185, #11519, #5151 ) ;
#2333 = DIRECTION ( 'NONE',  ( 1.000000000000000000, 0.000000000000000000, 0.000000000000000000 ) ) ;
#2334 = CARTESIAN_POINT ( 'NONE',  ( 34.69999999999998863, -85.00000000000000000, 79.39999999999999147 ) ) ;
#2335 = AXIS2_PLACEMENT_3D ( 'NONE', #1746, #18632, #6681 ) ;
#2336 =( GEOMETRIC_REPRESENTATION_CONTEXT ( 3 ) GLOBAL_UNCERTAINTY_ASSIGNED_CONTEXT ( ( #16464 ) ) GLOBAL_UNIT_ASSIGNED_CONTEXT ( ( #4219, #11038, #2638 ) ) REPRESENTATION_CONTEXT ( 'NONE', 'WORKASPACE' ) );
#2337 = CIRCLE ( 'NONE', #10916, 0.2999999999999947153 ) ;
#2338 = EDGE_LOOP ( 'NONE', ( #11303, #1294, #15011, #19894 ) ) ;
#2339 = FACE_OUTER_BOUND ( 'NONE', #12760, .T. ) ;
#2340 = ORIENTED_EDGE ( 'NONE', *, *, #18821, .F. ) ;
#2341 = ADVANCED_FACE ( 'NONE', ( #17894 ), #14529, .T. ) ;
#2342 = EDGE_LOOP ( 'NONE', ( #7454, #1231, #691, #11678, #15285, #9026, #12456, #21836, #19722, #10350, #14459, #1855 ) ) ;
#2343 = CARTESIAN_POINT ( 'NONE',  ( 17.95292532278785913, 34.11873716947361856, 42.50000000000000711 ) ) ;
#2344 = ORIENTED_EDGE ( 'NONE', *, *, #1542, .F. ) ;
#2345 = EDGE_LOOP ( 'NONE', ( #2284, #16505, #8213, #19046 ) ) ;
#2346 = AXIS2_PLACEMENT_3D ( 'NONE', #17140, #8866, #12095 ) ;
#2347 = EDGE_CURVE ( 'NONE', #4007, #19672, #16318, .T. ) ;
#2348 = CARTESIAN_POINT ( 'NONE',  ( 23.13130088652697225, -2.712279394122553366, 13.41537141447308379 ) ) ;
#2349 = ORIENTED_EDGE ( 'NONE', *, *, #7933, .T. ) ;
#2350 = FACE_OUTER_BOUND ( 'NONE', #12415, .T. ) ;
#2351 = AXIS2_PLACEMENT_3D ( 'NONE', #4186, #21210, #19741 ) ;
#2352 = AXIS2_PLACEMENT_3D ( 'NONE', #12890, #4402, #7893 ) ;
#2353 = AXIS2_PLACEMENT_3D ( 'NONE', #13359, #20312, #13789 ) ;
#2354 = LINE ( 'NONE', #8972, #8802 ) ;
#2355 = DIRECTION ( 'NONE',  ( 0.000000000000000000, 0.000000000000000000, 1.000000000000000000 ) ) ;
#2356 = DIRECTION ( 'NONE',  ( 0.000000000000000000, -1.000000000000000000, 0.000000000000000000 ) ) ;
#2357 = DIRECTION ( 'NONE',  ( 0.000000000000000000, 0.000000000000000000, 1.000000000000000000 ) ) ;
#2358 = DIRECTION ( 'NONE',  ( 0.000000000000000000, 0.000000000000000000, 1.000000000000000000 ) ) ;
#2359 = DIRECTION ( 'NONE',  ( 0.000000000000000000, -1.000000000000000000, 0.000000000000000000 ) ) ;
#2360 = CARTESIAN_POINT ( 'NONE',  ( -29.13662752439705272, 0.000000000000000000, 0.3000000000000016542 ) ) ;
#2361 = DIRECTION ( 'NONE',  ( -0.000000000000000000, -1.000000000000000000, -0.000000000000000000 ) ) ;
#2362 = AXIS2_PLACEMENT_3D ( 'NONE', #2476, #21182, #18010 ) ;
#2363 = AXIS2_PLACEMENT_3D ( 'NONE', #21658, #7669, #1156 ) ;
#2364 = VECTOR ( 'NONE', #13078, 1000.000000000000000 ) ;
#2365 = EDGE_CURVE ( 'NONE', #19005, #20280, #997, .T. ) ;
#2366 = EDGE_LOOP ( 'NONE', ( #5505, #10928, #15389, #10607 ) ) ;
#2367 = CIRCLE ( 'NONE', #10608, 0.5000000000000004441 ) ;
#2368 = CARTESIAN_POINT ( 'NONE',  ( 28.87540678000427619, 6.494748934539263274, 7.799999999999999822 ) ) ;
#2369 = DIRECTION ( 'NONE',  ( -1.000000000000000000, 0.000000000000000000, 0.000000000000000000 ) ) ;
#2370 = ORIENTED_EDGE ( 'NONE', *, *, #15780, .T. ) ;
#2371 = ORIENTED_EDGE ( 'NONE', *, *, #7376, .T. ) ;
#2372 = EDGE_CURVE ( 'NONE', #7310, #12793, #3657, .T. ) ;
#2373 = EDGE_CURVE ( 'NONE', #13948, #18889, #10442, .T. ) ;
#2374 = CIRCLE ( 'NONE', #8113, 0.05000000000000143219 ) ;
#2375 = AXIS2_PLACEMENT_3D ( 'NONE', #5897, #19531, #4212 ) ;
#2376 = AXIS2_PLACEMENT_3D ( 'NONE', #184, #1879, #20803 ) ;
#2377 = AXIS2_PLACEMENT_3D ( 'NONE', #13694, #1511, #21793 ) ;
#2378 = CYLINDRICAL_SURFACE ( 'NONE', #19245, 0.2500000000000002220 ) ;
#2379 = DIRECTION ( 'NONE',  ( -0.000000000000000000, -0.000000000000000000, -1.000000000000000000 ) ) ;
#2380 = CIRCLE ( 'NONE', #18833, 1.000000000000000888 ) ;
#2381 = VERTEX_POINT ( 'NONE', #6066 ) ;
#2382 = CARTESIAN_POINT ( 'NONE',  ( -35.00000000000000000, -84.70000000000001705, 1.500000000000000000 ) ) ;
#2383 = CARTESIAN_POINT ( 'NONE',  ( 23.32398829872514057, 3.528912754968628551, 13.50000000000000000 ) ) ;
#2384 = LINE ( 'NONE', #9216, #3630 ) ;
#2385 = CARTESIAN_POINT ( 'NONE',  ( 15.00584427753688921, 51.86868465798484351, 13.49999999999999645 ) ) ;
#2386 = CARTESIAN_POINT ( 'NONE',  ( -30.67540678000428045, 6.000000000000000000, 3.500000000000000000 ) ) ;
#2387 = CARTESIAN_POINT ( 'NONE',  ( -33.50000000000001421, 84.70000000000001705, 78.50000000000000000 ) ) ;
#2388 = ADVANCED_FACE ( 'NONE', ( #12852 ), #11499, .T. ) ;
#2389 = ORIENTED_EDGE ( 'NONE', *, *, #18129, .F. ) ;
#2390 = CARTESIAN_POINT ( 'NONE',  ( 1.724728116533979838, 43.31054587065082728, 45.66679706732590205 ) ) ;
#2391 = DIRECTION ( 'NONE',  ( -1.000000000000000000, 0.000000000000000000, 0.000000000000000000 ) ) ;
#2392 = VECTOR ( 'NONE', #20192, 1000.000000000000000 ) ;
#2393 = CARTESIAN_POINT ( 'NONE',  ( 4.127054932750481520, 32.93424481021354921, 7.321391277662001151 ) ) ;
#2394 = VERTEX_POINT ( 'NONE', #19698 ) ;
#2395 = CIRCLE ( 'NONE', #16685, 2.800000000000003819 ) ;
#2396 = CIRCLE ( 'NONE', #15594, 3.500000000000003109 ) ;
#2397 = ORIENTED_EDGE ( 'NONE', *, *, #7273, .F. ) ;
#2398 = ORIENTED_EDGE ( 'NONE', *, *, #10800, .T. ) ;
#2399 = CARTESIAN_POINT ( 'NONE',  ( -29.17540678000427690, -6.499884319688664647, 7.500000000000000000 ) ) ;
#2400 = DIRECTION ( 'NONE',  ( -1.000000000000000000, 0.000000000000000000, 0.000000000000000000 ) ) ;
#2401 = EDGE_LOOP ( 'NONE', ( #5803, #441, #4168, #11659 ) ) ;
#2402 = VECTOR ( 'NONE', #19412, 1000.000000000000000 ) ;
#2403 = DIRECTION ( 'NONE',  ( -1.224646799147353207E-16, -0.000000000000000000, -1.000000000000000000 ) ) ;
#2404 = EDGE_CURVE ( 'NONE', #7401, #9771, #16204, .T. ) ;
#2405 = EDGE_CURVE ( 'NONE', #17841, #2078, #2914, .T. ) ;
#2406 = ORIENTED_EDGE ( 'NONE', *, *, #17159, .F. ) ;
#2407 = DIRECTION ( 'NONE',  ( 1.000000000000000000, 3.543406725251269872E-15, -1.224646799147353207E-16 ) ) ;
#2408 =( BOUNDED_SURFACE ( )  B_SPLINE_SURFACE ( 3, 2, ( 
 ( #13740, #17003, #20600 ),
 ( #16662, #18689, #18349 ),
 ( #15001, #1675, #9974 ),
 ( #8518, #3476, #16784 ),
 ( #15333, #6623, #8298 ),
 ( #1453, #1795, #16897 ),
 ( #15102, #13422, #4936 ),
 ( #4, #8632, #6858 ) ),
 .UNSPECIFIED., .F., .F., .F. ) 
 B_SPLINE_SURFACE_WITH_KNOTS ( ( 4, 2, 2, 4 ),
 ( 3, 3 ),
 ( -1.016439536705160407E-20, 0.0002312589012449743479, 0.0004625178024899486958, 0.0009250356049798973915 ),
 ( 0.000000000000000000, 1.000000000000000000 ),
 .UNSPECIFIED. ) 
 GEOMETRIC_REPRESENTATION_ITEM ( )  RATIONAL_B_SPLINE_SURFACE ( (
 ( 1.000000000000000000, 0.7071067811865475727, 1.000000000000000000),
 ( 1.000000000000000000, 0.6819975405126383894, 1.000000000000000000),
 ( 1.000000000000000000, 0.6638073299468163491, 1.000000000000000000),
 ( 1.000000000000000000, 0.6387680821201728865, 1.000000000000000000),
 ( 1.000000000000000000, 0.6313903660824350395, 1.000000000000000000),
 ( 1.000000000000000000, 0.6152524581541630733, 1.000000000000000000),
 ( 1.000000000000000000, 0.6128152994388438302, 1.000000000000000000),
 ( 1.000000000000000000, 0.6123724356957929160, 1.000000000000000000) ) ) 
 REPRESENTATION_ITEM ( '' )  SURFACE ( )  );
#2409 = CARTESIAN_POINT ( 'NONE',  ( 15.21174975910707161, 41.81054587065082728, 68.25000000000000000 ) ) ;
#2410 = EDGE_CURVE ( 'NONE', #5908, #21506, #13293, .T. ) ;
#2411 = DIRECTION ( 'NONE',  ( 0.000000000000000000, -1.000000000000000000, 0.000000000000000000 ) ) ;
#2412 = CARTESIAN_POINT ( 'NONE',  ( 15.95292532278785913, 50.11873716947361856, 13.79999999999999893 ) ) ;
#2413 = AXIS2_PLACEMENT_3D ( 'NONE', #9609, #6150, #6371 ) ;
#2414 = AXIS2_PLACEMENT_3D ( 'NONE', #21482, #1189, #13279 ) ;
#2415 = VECTOR ( 'NONE', #16537, 1000.000000000000000 ) ;
#2416 = FACE_OUTER_BOUND ( 'NONE', #13489, .T. ) ;
#2417 = DIRECTION ( 'NONE',  ( -1.000000000000000000, -0.000000000000000000, 0.000000000000000000 ) ) ;
#2418 = ORIENTED_EDGE ( 'NONE', *, *, #4834, .F. ) ;
#2419 = DIRECTION ( 'NONE',  ( -1.000000000000000000, 0.000000000000000000, 0.000000000000000000 ) ) ;
#2420 = CARTESIAN_POINT ( 'NONE',  ( 14.96174975910705918, -51.86873716947361856, 14.00000000000000000 ) ) ;
#2421 = TOROIDAL_SURFACE ( 'NONE', #10294, 0.05000000000000000278, 0.05000000000000000278 ) ;
#2422 = DIRECTION ( 'NONE',  ( -1.000000000000000000, 0.000000000000000000, 0.000000000000000000 ) ) ;
#2423 = DIRECTION ( 'NONE',  ( 1.000000000000000000, 0.000000000000000000, 0.000000000000000000 ) ) ;
#2424 = ORIENTED_EDGE ( 'NONE', *, *, #17514, .F. ) ;
#2425 = CARTESIAN_POINT ( 'NONE',  ( -23.32398829872514057, 7.118794219358020148E-15, 13.79999999999999893 ) ) ;
#2426 = VECTOR ( 'NONE', #9563, 1000.000000000000000 ) ;
#2427 = AXIS2_PLACEMENT_3D ( 'NONE', #12238, #14035, #2069 ) ;
#2428 = ORIENTED_EDGE ( 'NONE', *, *, #11750, .T. ) ;
#2429 = CARTESIAN_POINT ( 'NONE',  ( -1.774728116533986544, 42.31054587065082728, 47.80876104995653719 ) ) ;
#2430 = CARTESIAN_POINT ( 'NONE',  ( -23.02398829872513275, -3.002822642624744631, 13.75715867294163353 ) ) ;
#2431 = ORIENTED_EDGE ( 'NONE', *, *, #17254, .F. ) ;
#2432 = ORIENTED_EDGE ( 'NONE', *, *, #3274, .T. ) ;
#2433 = FACE_OUTER_BOUND ( 'NONE', #11290, .T. ) ;
#2434 = DIRECTION ( 'NONE',  ( 1.000000000000000000, 0.000000000000000000, 0.000000000000000000 ) ) ;
#2435 = ADVANCED_FACE ( 'NONE', ( #19931 ), #4595, .T. ) ;
#2436 = DIRECTION ( 'NONE',  ( 0.000000000000000000, 0.000000000000000000, 1.000000000000000000 ) ) ;
#2437 = VECTOR ( 'NONE', #12468, 1000.000000000000000 ) ;
#2438 = CIRCLE ( 'NONE', #17793, 0.1000000000000028644 ) ;
#2439 = ORIENTED_EDGE ( 'NONE', *, *, #11128, .T. ) ;
#2440 = CIRCLE ( 'NONE', #6018, 0.09999999999999939493 ) ;
#2441 = ORIENTED_EDGE ( 'NONE', *, *, #765, .T. ) ;
#2442 = AXIS2_PLACEMENT_3D ( 'NONE', #7208, #19282, #3959 ) ;
#2443 = VECTOR ( 'NONE', #20678, 1000.000000000000000 ) ;
#2444 = EDGE_CURVE ( 'NONE', #15889, #5258, #10447, .T. ) ;
#2445 = ORIENTED_EDGE ( 'NONE', *, *, #1464, .F. ) ;
#2446 = CARTESIAN_POINT ( 'NONE',  ( -29.13662752439705272, 0.000000000000000000, 13.19999999999999929 ) ) ;
#2447 = CARTESIAN_POINT ( 'NONE',  ( 34.39999999999998437, 85.00000000000000000, 79.39999999999999147 ) ) ;
#2448 = DIRECTION ( 'NONE',  ( -0.000000000000000000, 1.000000000000000000, -0.000000000000000000 ) ) ;
#2449 = CARTESIAN_POINT ( 'NONE',  ( -25.37540678000427263, 68.74634676501045760, 3.799999999999999822 ) ) ;
#2450 = LINE ( 'NONE', #17769, #604 ) ;
#2451 = ORIENTED_EDGE ( 'NONE', *, *, #14528, .F. ) ;
#2452 = AXIS2_PLACEMENT_3D ( 'NONE', #4676, #14391, #7929 ) ;
#2453 = CARTESIAN_POINT ( 'NONE',  ( 14.66918480534031666, 51.92478805997377123, 13.49999999999999645 ) ) ;
#2454 = AXIS2_PLACEMENT_3D ( 'NONE', #12944, #9615, #21488 ) ;
#2455 = DIRECTION ( 'NONE',  ( -0.000000000000000000, -0.000000000000000000, 1.000000000000000000 ) ) ;
#2456 = ORIENTED_EDGE ( 'NONE', *, *, #172, .T. ) ;
#2457 = ADVANCED_FACE ( 'NONE', ( #14649 ), #11409, .T. ) ;
#2458 = FACE_OUTER_BOUND ( 'NONE', #2264, .T. ) ;
#2459 = EDGE_LOOP ( 'NONE', ( #19977, #1433, #19535, #7625 ) ) ;
#2460 = ADVANCED_FACE ( 'NONE', ( #12961 ), #19023, .T. ) ;
#2461 = ORIENTED_EDGE ( 'NONE', *, *, #10506, .F. ) ;
#2462 = ORIENTED_EDGE ( 'NONE', *, *, #7530, .T. ) ;
#2463 = DIRECTION ( 'NONE',  ( 0.000000000000000000, 0.000000000000000000, 1.000000000000000000 ) ) ;
#2464 = PRODUCT_CONTEXT ( 'NONE', #419, 'mechanical' ) ;
#2465 = ORIENTED_EDGE ( 'NONE', *, *, #11344, .F. ) ;
#2466 = CIRCLE ( 'NONE', #9259, 0.5000000000000004441 ) ;
#2467 = VERTEX_POINT ( 'NONE', #21997 ) ;
#2468 = AXIS2_PLACEMENT_3D ( 'NONE', #13944, #20689, #20795 ) ;
#2469 = VERTEX_POINT ( 'NONE', #7004 ) ;
#2470 = DIRECTION ( 'NONE',  ( 0.000000000000000000, -1.000000000000000000, 0.000000000000000000 ) ) ;
#2471 = AXIS2_PLACEMENT_3D ( 'NONE', #16263, #947, #14604 ) ;
#2472 = ORIENTED_EDGE ( 'NONE', *, *, #11020, .F. ) ;
#2473 = TOROIDAL_SURFACE ( 'NONE', #8206, 1.750000000000000000, 0.2500000000000000000 ) ;
#2474 = CARTESIAN_POINT ( 'NONE',  ( 15.95292532278785913, -32.11873716947361856, 42.50000000000000711 ) ) ;
#2475 = DIRECTION ( 'NONE',  ( 0.000000000000000000, -1.000000000000000000, 0.000000000000000000 ) ) ;
#2476 = CARTESIAN_POINT ( 'NONE',  ( -21.92816239687475743, 42.46645089659918426, 68.25000000000000000 ) ) ;
#2477 = ADVANCED_FACE ( 'NONE', ( #5208 ), #8342, .T. ) ;
#2478 = CARTESIAN_POINT ( 'NONE',  ( 15.21174975910707161, 42.11054587065083155, 13.50000000000000000 ) ) ;
#2479 = CARTESIAN_POINT ( 'NONE',  ( -33.80000000000001847, 84.70000000000001705, 80.00000000000000000 ) ) ;
#2480 = DIRECTION ( 'NONE',  ( 0.000000000000000000, 0.000000000000000000, 1.000000000000000000 ) ) ;
#2481 = DIRECTION ( 'NONE',  ( -1.000000000000000000, 0.000000000000000000, -0.000000000000000000 ) ) ;
#2482 = ADVANCED_FACE ( 'NONE', ( #13363 ), #13690, .F. ) ;
#2483 = CARTESIAN_POINT ( 'NONE',  ( -21.92816239687475743, 42.46645089659918426, 13.50000000000000000 ) ) ;
#2484 = AXIS2_PLACEMENT_3D ( 'NONE', #11592, #18425, #15075 ) ;
#2485 = CIRCLE ( 'NONE', #21091, 0.5000000000000004441 ) ;
#2486 = VECTOR ( 'NONE', #20491, 1000.000000000000000 ) ;
#2487 = EDGE_LOOP ( 'NONE', ( #20914, #11222, #7918, #18871 ) ) ;
#2488 = ORIENTED_EDGE ( 'NONE', *, *, #15415, .T. ) ;
#2489 = DIRECTION ( 'NONE',  ( 0.000000000000000000, -0.000000000000000000, -1.000000000000000000 ) ) ;
#2490 = VERTEX_POINT ( 'NONE', #11902 ) ;
#2491 = ADVANCED_FACE ( 'NONE', ( #12009 ), #8779, .T. ) ;
#2492 = CIRCLE ( 'NONE', #2484, 0.04999999999999991257 ) ;
#2493 = DIRECTION ( 'NONE',  ( 0.000000000000000000, 0.000000000000000000, 1.000000000000000000 ) ) ;
#2494 = VECTOR ( 'NONE', #20863, 1000.000000000000000 ) ;
#2495 = CARTESIAN_POINT ( 'NONE',  ( -9.178906393579033818, 42.46645089659918426, 1067.751649863784678 ) ) ;
#2496 = VERTEX_POINT ( 'NONE', #18515 ) ;
#2497 = LINE ( 'NONE', #2382, #20041 ) ;
#2498 = CARTESIAN_POINT ( 'NONE',  ( -31.31859531322107060, 84.19398174988410233, 13.75000000000000000 ) ) ;
#2499 = CARTESIAN_POINT ( 'NONE',  ( -28.71290943744531177, 6.649236572130504896, 13.47739020623642325 ) ) ;
#2500 = FACE_OUTER_BOUND ( 'NONE', #6431, .T. ) ;
#2501 = PLANE ( 'NONE',  #2352 ) ;
#2502 = EDGE_CURVE ( 'NONE', #17966, #9603, #6418, .T. ) ;
#2503 = VERTEX_POINT ( 'NONE', #3307 ) ;
#2504 = CARTESIAN_POINT ( 'NONE',  ( 28.86382559268571057, -6.505889654322387194, 13.29319881794719294 ) ) ;
#2505 = DIRECTION ( 'NONE',  ( -0.000000000000000000, 1.000000000000000000, -0.000000000000000000 ) ) ;
#2506 = EDGE_CURVE ( 'NONE', #17693, #22137, #2466, .T. ) ;
#2507 = DIRECTION ( 'NONE',  ( -0.000000000000000000, -0.000000000000000000, -1.000000000000000000 ) ) ;
#2508 = EDGE_LOOP ( 'NONE', ( #3186, #12936, #4883, #8474 ) ) ;
#2509 = ORIENTED_EDGE ( 'NONE', *, *, #21702, .F. ) ;
#2510 = ORIENTED_EDGE ( 'NONE', *, *, #10171, .T. ) ;
#2511 = DIRECTION ( 'NONE',  ( 0.000000000000000000, -0.000000000000000000, 1.000000000000000000 ) ) ;
#2512 = TOROIDAL_SURFACE ( 'NONE', #18960, 4.700000000000004619, 0.2999999999999999889 ) ;
#2513 = DIRECTION ( 'NONE',  ( 0.000000000000000000, 1.000000000000000000, -0.000000000000000000 ) ) ;
#2514 = ORIENTED_EDGE ( 'NONE', *, *, #2945, .T. ) ;
#2515 = CIRCLE ( 'NONE', #10749, 0.2499999999999985012 ) ;
#2516 = DIRECTION ( 'NONE',  ( 0.000000000000000000, 0.000000000000000000, 1.000000000000000000 ) ) ;
#2517 = ORIENTED_EDGE ( 'NONE', *, *, #10993, .F. ) ;
#2518 = CARTESIAN_POINT ( 'NONE',  ( -31.26086011588027347, 83.95073979834609190, 13.75000000000000000 ) ) ;
#2519 = DIRECTION ( 'NONE',  ( 1.000000000000000000, 0.000000000000000000, 0.000000000000000000 ) ) ;
#2520 = EDGE_CURVE ( 'NONE', #706, #13756, #8575, .T. ) ;
#2521 = LINE ( 'NONE', #9027, #21027 ) ;
#2522 = DIRECTION ( 'NONE',  ( 0.000000000000000000, 0.000000000000000000, 1.000000000000000000 ) ) ;
#2523 = DIRECTION ( 'NONE',  ( -0.000000000000000000, -0.000000000000000000, -1.000000000000000000 ) ) ;
#2524 = CYLINDRICAL_SURFACE ( 'NONE', #14475, 0.04999999999999991257 ) ;
#2525 = ORIENTED_EDGE ( 'NONE', *, *, #14675, .F. ) ;
#2526 = CYLINDRICAL_SURFACE ( 'NONE', #5262, 0.5000000000000004441 ) ;
#2527 = LINE ( 'NONE', #2420, #4970 ) ;
#2528 = VECTOR ( 'NONE', #6351, 1000.000000000000000 ) ;
#2529 = AXIS2_PLACEMENT_3D ( 'NONE', #19784, #6367, #9377 ) ;
#2530 = CARTESIAN_POINT ( 'NONE',  ( 0.000000000000000000, -51.61873716947361856, 14.00000000000000000 ) ) ;
#2531 = DIRECTION ( 'NONE',  ( -0.000000000000000000, 1.000000000000000000, -0.000000000000000000 ) ) ;
#2532 = EDGE_LOOP ( 'NONE', ( #11726, #11430, #19783, #12810 ) ) ;
#2533 = LINE ( 'NONE', #14718, #10552 ) ;
#2534 = FACE_OUTER_BOUND ( 'NONE', #5674, .T. ) ;
#2535 = ADVANCED_FACE ( 'NONE', ( #11683 ), #1938, .T. ) ;
#2536 = VERTEX_POINT ( 'NONE', #3531 ) ;
#2537 = DIRECTION ( 'NONE',  ( 0.000000000000000000, 1.000000000000000000, 0.000000000000000000 ) ) ;
#2538 = EDGE_CURVE ( 'NONE', #7977, #6397, #15384, .T. ) ;
#2539 = CARTESIAN_POINT ( 'NONE',  ( 14.96174975910705918, 50.19799549595485644, 13.75000000000000000 ) ) ;
#2540 = VERTEX_POINT ( 'NONE', #6676 ) ;
#2541 = ORIENTED_EDGE ( 'NONE', *, *, #3942, .T. ) ;
#2542 = DIRECTION ( 'NONE',  ( 1.000000000000000000, 0.000000000000000000, 0.000000000000000000 ) ) ;
#2544 = ADVANCED_FACE ( 'NONE', ( #1735 ), #8683, .T. ) ;
#2543 = CARTESIAN_POINT ( 'NONE',  ( 25.37540678000427263, 68.74634676501045760, 7.200000000000000178 ) ) ;
#2545 = CARTESIAN_POINT ( 'NONE',  ( 9.641460742840918030, -32.93424481021354921, 68.50000000000000000 ) ) ;
#2546 = AXIS2_PLACEMENT_3D ( 'NONE', #11506, #17068, #6384 ) ;
#2547 = ORIENTED_EDGE ( 'NONE', *, *, #570, .T. ) ;
#2548 = AXIS2_PLACEMENT_3D ( 'NONE', #4315, #9346, #11349 ) ;
#2549 = ORIENTED_EDGE ( 'NONE', *, *, #6283, .T. ) ;
#2550 = EDGE_CURVE ( 'NONE', #10124, #21689, #56, .T. ) ;
#2551 = ORIENTED_EDGE ( 'NONE', *, *, #9413, .T. ) ;
#2552 = DIRECTION ( 'NONE',  ( 0.000000000000000000, 1.000000000000000000, -0.000000000000000000 ) ) ;
#2553 = VECTOR ( 'NONE', #19074, 1000.000000000000000 ) ;
#2554 = CARTESIAN_POINT ( 'NONE',  ( 15.21174975910705918, 41.81054587065082728, 13.50000000000000000 ) ) ;
#2555 = CARTESIAN_POINT ( 'NONE',  ( -32.29156311937310164, 83.96304096052089960, 68.50000000000000000 ) ) ;
#2556 = DIRECTION ( 'NONE',  ( -1.000000000000000000, -0.000000000000000000, 0.000000000000000000 ) ) ;
#2557 = AXIS2_PLACEMENT_3D ( 'NONE', #13671, #6770, #20514 ) ;
#2558 = VECTOR ( 'NONE', #11883, 1000.000000000000000 ) ;
#2559 = FACE_OUTER_BOUND ( 'NONE', #8880, .T. ) ;
#2560 = PLANE ( 'NONE',  #19605 ) ;
#2561 = ORIENTED_EDGE ( 'NONE', *, *, #2948, .F. ) ;
#2562 = DIRECTION ( 'NONE',  ( 0.000000000000000000, -0.000000000000000000, -1.000000000000000000 ) ) ;
#2563 = CARTESIAN_POINT ( 'NONE',  ( -8.378839169841056034, 43.00645089659919051, 68.06527860057354928 ) ) ;
#2564 = EDGE_CURVE ( 'NONE', #5916, #5378, #8451, .T. ) ;
#2565 = CARTESIAN_POINT ( 'NONE',  ( -14.66174975910705136, -51.76873716947361714, 13.50000000000000000 ) ) ;
#2567 = EDGE_CURVE ( 'NONE', #9364, #11183, #3278, .T. ) ;
#2566 = DIRECTION ( 'NONE',  ( 0.000000000000000000, -0.000000000000000000, -1.000000000000000000 ) ) ;
#2568 = CARTESIAN_POINT ( 'NONE',  ( -31.50000000000002132, -72.00000000000001421, 1.800000000000000044 ) ) ;
#2569 = ORIENTED_EDGE ( 'NONE', *, *, #17322, .F. ) ;
#2570 = VECTOR ( 'NONE', #21005, 1000.000000000000000 ) ;
#2571 = VERTEX_POINT ( 'NONE', #17058 ) ;
#2572 = CARTESIAN_POINT ( 'NONE',  ( -14.96174975910705207, 42.31054587065082728, 68.25000000000000000 ) ) ;
#2573 = CONTEXT_DEPENDENT_SHAPE_REPRESENTATION ( #15715, #20188 ) ;
#2574 = AXIS2_PLACEMENT_3D ( 'NONE', #9858, #10312, #18459 ) ;
#2575 = ORIENTED_EDGE ( 'NONE', *, *, #11279, .T. ) ;
#2576 = AXIS2_PLACEMENT_3D ( 'NONE', #11286, #18238, #7626 ) ;
#2577 = AXIS2_PLACEMENT_3D ( 'NONE', #13536, #5152, #17320 ) ;
#2578 = ORIENTED_EDGE ( 'NONE', *, *, #10121, .F. ) ;
#2579 = VECTOR ( 'NONE', #16443, 1000.000000000000000 ) ;
#2580 = DIRECTION ( 'NONE',  ( 0.000000000000000000, 0.000000000000000000, -1.000000000000000000 ) ) ;
#2581 = CARTESIAN_POINT ( 'NONE',  ( 15.95292532278785913, 32.11873716947361856, 68.50000000000000000 ) ) ;
#2582 = ORIENTED_EDGE ( 'NONE', *, *, #17921, .F. ) ;
#2583 = DIRECTION ( 'NONE',  ( -0.000000000000000000, -0.000000000000000000, -1.000000000000000000 ) ) ;
#2584 = ORIENTED_EDGE ( 'NONE', *, *, #6753, .F. ) ;
#2585 = EDGE_CURVE ( 'NONE', #11808, #6249, #21864, .T. ) ;
#2586 = CARTESIAN_POINT ( 'NONE',  ( 25.37540678000427263, -63.74634676501045050, 13.19999999999999929 ) ) ;
#2587 = CARTESIAN_POINT ( 'NONE',  ( 8.641460742840918030, -33.93424481021354921, 68.00000000000000000 ) ) ;
#2588 = EDGE_CURVE ( 'NONE', #1357, #6635, #4874, .T. ) ;
#2589 = DIRECTION ( 'NONE',  ( 0.000000000000000000, -1.000000000000000000, 0.000000000000000000 ) ) ;
#2590 = VECTOR ( 'NONE', #18925, 1000.000000000000000 ) ;
#2591 = SPHERICAL_SURFACE ( 'NONE', #1833, 0.5000000000000000000 ) ;
#2592 = AXIS2_PLACEMENT_3D ( 'NONE', #21206, #4073, #477 ) ;
#2593 = CARTESIAN_POINT ( 'NONE',  ( -1.774728116533986766, 43.26054587065083012, 24.00000000000000000 ) ) ;
#2594 = CARTESIAN_POINT ( 'NONE',  ( -9.718906393579157310, 41.42245079618239600, 68.06527860057354928 ) ) ;
#2595 = DIRECTION ( 'NONE',  ( -1.224646799147353207E-16, 0.000000000000000000, -1.000000000000000000 ) ) ;
#2596 = FACE_OUTER_BOUND ( 'NONE', #20416, .T. ) ;
#2597 = ORIENTED_EDGE ( 'NONE', *, *, #8247, .T. ) ;
#2598 = CYLINDRICAL_SURFACE ( 'NONE', #4220, 0.05000000000000143219 ) ;
#2599 = VECTOR ( 'NONE', #4963, 1000.000000000000000 ) ;
#2600 = FACE_OUTER_BOUND ( 'NONE', #13275, .T. ) ;
#2601 = ORIENTED_EDGE ( 'NONE', *, *, #4453, .T. ) ;
#2602 = DIRECTION ( 'NONE',  ( 0.000000000000000000, 0.000000000000000000, 1.000000000000000000 ) ) ;
#2603 = EDGE_CURVE ( 'NONE', #12236, #6333, #19002, .T. ) ;
#2604 = DIRECTION ( 'NONE',  ( -1.000000000000000000, 0.000000000000000000, -6.123233995736764803E-17 ) ) ;
#2605 = VERTEX_POINT ( 'NONE', #17379 ) ;
#2606 = DIRECTION ( 'NONE',  ( 2.388292521039847891E-16, 0.000000000000000000, 1.000000000000000000 ) ) ;
#2607 = DIRECTION ( 'NONE',  ( 0.000000000000000000, 0.000000000000000000, 1.000000000000000000 ) ) ;
#2608 = CARTESIAN_POINT ( 'NONE',  ( 14.90249074828138198, 52.32070855728485981, 13.50000000000000000 ) ) ;
#2609 = DIRECTION ( 'NONE',  ( 1.000000000000000000, 0.000000000000000000, 0.000000000000000000 ) ) ;
#2610 = DIRECTION ( 'NONE',  ( -1.000000000000000000, 0.000000000000000000, 0.000000000000000000 ) ) ;
#2611 = ORIENTED_EDGE ( 'NONE', *, *, #3078, .T. ) ;
#2612 = DIRECTION ( 'NONE',  ( 0.000000000000000000, -1.000000000000000000, 0.000000000000000000 ) ) ;
#2613 = CARTESIAN_POINT ( 'NONE',  ( 17.45292532278785913, 50.11873716947361856, 14.00000000000000000 ) ) ;
#2614 = EDGE_LOOP ( 'NONE', ( #19265, #8650, #9650, #7642, #3004 ) ) ;
#2615 = ORIENTED_EDGE ( 'NONE', *, *, #19798, .T. ) ;
#2616 = ORIENTED_EDGE ( 'NONE', *, *, #5816, .T. ) ;
#2617 = CARTESIAN_POINT ( 'NONE',  ( 14.96243083687292597, 51.84435441965536029, 13.82657707279502013 ) ) ;
#2618 = CARTESIAN_POINT ( 'NONE',  ( 15.21174975910705918, -51.86873716947361856, 13.05380965755522737 ) ) ;
#2619 = ORIENTED_EDGE ( 'NONE', *, *, #3524, .F. ) ;
#2620 = EDGE_CURVE ( 'NONE', #4038, #444, #16841, .T. ) ;
#2621 = DIRECTION ( 'NONE',  ( -0.000000000000000000, 1.000000000000000000, 0.000000000000000000 ) ) ;
#2622 = ORIENTED_EDGE ( 'NONE', *, *, #9442, .T. ) ;
#2623 = FACE_OUTER_BOUND ( 'NONE', #3403, .T. ) ;
#2624 = CARTESIAN_POINT ( 'NONE',  ( 15.95292532278785913, 51.61873716947361856, 13.50000000000000000 ) ) ;
#2625 = EDGE_CURVE ( 'NONE', #4860, #6694, #15765, .T. ) ;
#2626 = EDGE_CURVE ( 'NONE', #22005, #6717, #2051, .T. ) ;
#2627 = CARTESIAN_POINT ( 'NONE',  ( 23.02398829872513986, -2.157133568460768647, 13.19999999999999929 ) ) ;
#2628 = CARTESIAN_POINT ( 'NONE',  ( 1.724728116533979838, 42.36054587065083155, 33.71679706732590631 ) ) ;
#2629 = CARTESIAN_POINT ( 'NONE',  ( 14.96174975910707161, 50.19799549595485644, 68.25000000000000000 ) ) ;
#2630 = DIRECTION ( 'NONE',  ( 1.000000000000000000, 0.000000000000000000, 0.000000000000000000 ) ) ;
#2631 = ORIENTED_EDGE ( 'NONE', *, *, #9324, .T. ) ;
#2632 = LINE ( 'NONE', #18187, #8461 ) ;
#2633 = CARTESIAN_POINT ( 'NONE',  ( -27.67540678000428400, -10.94079601157914716, 13.50000000000000000 ) ) ;
#2634 = AXIS2_PLACEMENT_3D ( 'NONE', #8015, #837, #14816 ) ;
#2635 = DIRECTION ( 'NONE',  ( 1.000000000000000000, 0.000000000000000000, 1.734723475976786140E-16 ) ) ;
#2636 = DIRECTION ( 'NONE',  ( -1.000000000000000000, 0.000000000000000000, 0.000000000000000000 ) ) ;
#2637 = ORIENTED_EDGE ( 'NONE', *, *, #1108, .T. ) ;
#2638 =( NAMED_UNIT ( * ) SI_UNIT ( $, .STERADIAN. ) SOLID_ANGLE_UNIT ( ) );
#2639 = DIRECTION ( 'NONE',  ( -1.000000000000000000, -3.387630566026860322E-15, 1.224646799147353207E-16 ) ) ;
#2640 = ORIENTED_EDGE ( 'NONE', *, *, #700, .F. ) ;
#2641 = DIRECTION ( 'NONE',  ( -0.000000000000000000, -1.000000000000000000, -0.000000000000000000 ) ) ;
#2642 = CIRCLE ( 'NONE', #21237, 0.1000000000000028644 ) ;
#2643 = DIRECTION ( 'NONE',  ( 0.000000000000000000, 1.000000000000000000, 0.000000000000000000 ) ) ;
#2644 = ORIENTED_EDGE ( 'NONE', *, *, #224, .F. ) ;
#2645 = AXIS2_PLACEMENT_3D ( 'NONE', #11903, #22123, #9909 ) ;
#2646 = EDGE_LOOP ( 'NONE', ( #20927, #13409, #19193, #18001 ) ) ;
#2647 = CARTESIAN_POINT ( 'NONE',  ( -15.21174975910705029, 52.10286008774955491, 13.87500000000000000 ) ) ;
#2648 = EDGE_CURVE ( 'NONE', #13584, #8339, #17567, .T. ) ;
#2649 = FACE_OUTER_BOUND ( 'NONE', #3275, .T. ) ;
#2650 = ORIENTED_EDGE ( 'NONE', *, *, #22050, .T. ) ;
#2651 = ORIENTED_EDGE ( 'NONE', *, *, #17785, .F. ) ;
#2652 = LINE ( 'NONE', #18210, #9318 ) ;
#2653 = EDGE_CURVE ( 'NONE', #1327, #5533, #8894, .T. ) ;
#2654 = ORIENTED_EDGE ( 'NONE', *, *, #6389, .F. ) ;
#2655 = CARTESIAN_POINT ( 'NONE',  ( -23.02398829872514696, -2.211005166399017341, 13.20000000000005969 ) ) ;
#2656 = EDGE_CURVE ( 'NONE', #19855, #19467, #17199, .T. ) ;
#2657 = DIRECTION ( 'NONE',  ( 0.000000000000000000, 0.000000000000000000, -1.000000000000000000 ) ) ;
#2658 = DIRECTION ( 'NONE',  ( -0.000000000000000000, 1.000000000000000000, -0.000000000000000000 ) ) ;
#2659 = EDGE_CURVE ( 'NONE', #7877, #12714, #12448, .T. ) ;
#2660 = CARTESIAN_POINT ( 'NONE',  ( 0.000000000000000000, 38.74634676501045760, 42.50000000000000000 ) ) ;
#2661 = DIRECTION ( 'NONE',  ( 1.788744114411106313E-17, 1.000000000000000000, 1.095289877103613968E-33 ) ) ;
#2662 = LINE ( 'NONE', #9163, #8878 ) ;
#2663 = VERTEX_POINT ( 'NONE', #2498 ) ;
#2664 = DIRECTION ( 'NONE',  ( 1.000000000000000000, 0.000000000000000000, 0.000000000000000000 ) ) ;
#2665 = CYLINDRICAL_SURFACE ( 'NONE', #4266, 0.5999999999999999778 ) ;
#2666 = DIRECTION ( 'NONE',  ( 1.000000000000000000, 0.000000000000000000, 0.000000000000000000 ) ) ;
#2667 = PLANE ( 'NONE',  #18908 ) ;
#2668 = EDGE_CURVE ( 'NONE', #21435, #13945, #12322, .T. ) ;
#2669 = CARTESIAN_POINT ( 'NONE',  ( -1.774728116533986766, 43.26054587065083012, 37.66679706732590915 ) ) ;
#2670 = VERTEX_POINT ( 'NONE', #19181 ) ;
#2671 = ORIENTED_EDGE ( 'NONE', *, *, #16402, .T. ) ;
#2672 = AXIS2_PLACEMENT_3D ( 'NONE', #21976, #13451, #20291 ) ;
#2673 = CYLINDRICAL_SURFACE ( 'NONE', #4954, 2.000000000000000000 ) ;
#2674 = ORIENTED_EDGE ( 'NONE', *, *, #20183, .T. ) ;
#2675 = CARTESIAN_POINT ( 'NONE',  ( -23.61959064016851073, 45.26242829375641463, 68.25000000000000000 ) ) ;
#2676 = DIRECTION ( 'NONE',  ( 0.000000000000000000, 0.000000000000000000, 1.000000000000000000 ) ) ;
#2677 = ORIENTED_EDGE ( 'NONE', *, *, #14438, .T. ) ;
#2678 = CARTESIAN_POINT ( 'NONE',  ( -24.43662752439705343, 0.000000000000000000, 3.799999999999999822 ) ) ;
#2679 = EDGE_CURVE ( 'NONE', #3260, #11867, #18633, .T. ) ;
#2680 = ORIENTED_EDGE ( 'NONE', *, *, #1292, .F. ) ;
#2681 = ADVANCED_FACE ( 'NONE', ( #2165 ), #7439, .T. ) ;
#2682 = DIRECTION ( 'NONE',  ( -1.000000000000000000, 0.000000000000000000, 0.000000000000000000 ) ) ;
#2683 = FACE_OUTER_BOUND ( 'NONE', #14585, .T. ) ;
#2684 = LINE ( 'NONE', #9302, #19885 ) ;
#2685 = AXIS2_PLACEMENT_3D ( 'NONE', #8692, #8902, #14029 ) ;
#2686 = COLOUR_RGB ( '', 0.31764706, 0.68627451, 0.89019608) ;
#2687 = LINE ( 'NONE', #9519, #1106 ) ;
#2688 = DIRECTION ( 'NONE',  ( -1.000000000000000000, 0.000000000000000000, -6.123233995736764803E-17 ) ) ;
#2689 = CARTESIAN_POINT ( 'NONE',  ( -1.774728116533986766, 42.31054587065082728, 12.00000000000000000 ) ) ;
#2690 = LINE ( 'NONE', #5755, #13005 ) ;
#2691 = VERTEX_POINT ( 'NONE', #15806 ) ;
#2692 = CARTESIAN_POINT ( 'NONE',  ( -15.21174975910705207, 51.61873716947361856, 68.50000000000000000 ) ) ;
#2693 = CYLINDRICAL_SURFACE ( 'NONE', #15621, 1.999999999999991340 ) ;
#2694 = ORIENTED_EDGE ( 'NONE', *, *, #7835, .F. ) ;
#2695 = ORIENTED_EDGE ( 'NONE', *, *, #19331, .T. ) ;
#2696 = CARTESIAN_POINT ( 'NONE',  ( -1.724728116533986721, 42.36054587065083155, 41.76679706732590347 ) ) ;
#2697 =( LENGTH_UNIT ( ) NAMED_UNIT ( * ) SI_UNIT ( .MILLI., .METRE. ) );
#2699 = EDGE_CURVE ( 'NONE', #13403, #17454, #10422, .T. ) ;
#2698 = DIRECTION ( 'NONE',  ( -0.000000000000000000, -0.000000000000000000, 1.000000000000000000 ) ) ;
#2700 = EDGE_LOOP ( 'NONE', ( #15288, #10930, #20717, #4285 ) ) ;
#2701 = AXIS2_PLACEMENT_3D ( 'NONE', #7085, #13882, #447 ) ;
#2702 = AXIS2_PLACEMENT_3D ( 'NONE', #15585, #10564, #17382 ) ;
#2703 = AXIS2_PLACEMENT_3D ( 'NONE', #2302, #7579, #3894 ) ;
#2704 = ORIENTED_EDGE ( 'NONE', *, *, #21393, .T. ) ;
#2705 = ORIENTED_EDGE ( 'NONE', *, *, #14543, .F. ) ;
#2706 = EDGE_CURVE ( 'NONE', #6037, #15847, #8637, .T. ) ;
#2707 =( REPRESENTATION_RELATIONSHIP ('NONE','NONE', #561, #6277 ) REPRESENTATION_RELATIONSHIP_WITH_TRANSFORMATION ( #5737 )SHAPE_REPRESENTATION_RELATIONSHIP( ) );
#2708 = CARTESIAN_POINT ( 'NONE',  ( 0.000000000000000000, -42.11054587065083155, 13.79999999999999893 ) ) ;
#2709 = VECTOR ( 'NONE', #13004, 1000.000000000000000 ) ;
#2710 = CARTESIAN_POINT ( 'NONE',  ( 30.49999999999999645, -123.9599366953518711, 0.3000000000000033751 ) ) ;
#2711 = AXIS2_PLACEMENT_3D ( 'NONE', #1911, #19150, #7192 ) ;
#2712 = ORIENTED_EDGE ( 'NONE', *, *, #19288, .F. ) ;
#2713 = FACE_OUTER_BOUND ( 'NONE', #8196, .T. ) ;
#2714 = FACE_OUTER_BOUND ( 'NONE', #14498, .T. ) ;
#2715 = CARTESIAN_POINT ( 'NONE',  ( 15.16923466928735742, 52.00603548408893317, 13.50000000000000000 ) ) ;
#2716 = CARTESIAN_POINT ( 'NONE',  ( 9.141460742840918030, -32.93424481021354921, 42.50000000000000000 ) ) ;
#2717 = CARTESIAN_POINT ( 'NONE',  ( -24.69594744299175915, 42.46645089659918426, 13.50000000000000000 ) ) ;
#2718 = CIRCLE ( 'NONE', #16284, 0.2500000000000002220 ) ;
#2719 = ORIENTED_EDGE ( 'NONE', *, *, #1861, .T. ) ;
#2720 = DIRECTION ( 'NONE',  ( -1.000000000000000000, 0.000000000000000000, -0.000000000000000000 ) ) ;
#2721 = DIRECTION ( 'NONE',  ( 0.000000000000000000, 0.000000000000000000, 1.000000000000000000 ) ) ;
#2722 = VERTEX_POINT ( 'NONE', #17606 ) ;
#2723 = ORIENTED_EDGE ( 'NONE', *, *, #1173, .F. ) ;
#2724 = ORIENTED_EDGE ( 'NONE', *, *, #4967, .T. ) ;
#2725 = DIRECTION ( 'NONE',  ( 0.000000000000000000, 0.000000000000000000, -1.000000000000000000 ) ) ;
#2727 = EDGE_CURVE ( 'NONE', #10373, #17848, #10887, .T. ) ;
#2726 = CARTESIAN_POINT ( 'NONE',  ( 23.32398829872514412, -3.528912754968634768, 13.50000000000000000 ) ) ;
#2728 = VERTEX_POINT ( 'NONE', #5871 ) ;
#2729 = EDGE_CURVE ( 'NONE', #1516, #1986, #2384, .T. ) ;
#2730 = TOROIDAL_SURFACE ( 'NONE', #6702, 1.750000000000000000, 0.2500000000000000000 ) ;
#2731 = AXIS2_PLACEMENT_3D ( 'NONE', #21669, #1392, #21893 ) ;
#2732 = AXIS2_PLACEMENT_3D ( 'NONE', #4775, #18308, #8458 ) ;
#2733 = CARTESIAN_POINT ( 'NONE',  ( -19.16037735075775217, 42.46645089659918426, 68.25000000000000000 ) ) ;
#2734 = AXIS2_PLACEMENT_3D ( 'NONE', #9850, #1552, #3250 ) ;
#2735 = ORIENTED_EDGE ( 'NONE', *, *, #960, .F. ) ;
#2736 = LINE ( 'NONE', #9571, #9666 ) ;
#2737 = AXIS2_PLACEMENT_3D ( 'NONE', #6294, #796, #14432 ) ;
#2738 = CARTESIAN_POINT ( 'NONE',  ( -8.149501154770145916, 43.00645089659919051, 70.88527860057354246 ) ) ;
#2739 = DIRECTION ( 'NONE',  ( -1.000000000000000000, -0.000000000000000000, -0.000000000000000000 ) ) ;
#2740 = DIRECTION ( 'NONE',  ( 0.000000000000000000, 0.000000000000000000, 1.000000000000000000 ) ) ;
#2741 = DIRECTION ( 'NONE',  ( 0.000000000000000000, 0.000000000000000000, 1.000000000000000000 ) ) ;
#2742 = DIRECTION ( 'NONE',  ( 1.000000000000000000, 0.000000000000000000, 0.000000000000000000 ) ) ;
#2743 = VERTEX_POINT ( 'NONE', #20761 ) ;
#2744 = DIRECTION ( 'NONE',  ( -1.000000000000000000, 0.000000000000000000, 0.000000000000000000 ) ) ;
#2745 = CARTESIAN_POINT ( 'NONE',  ( -1.824728116533986810, 42.36054587065083155, 49.71679706732589921 ) ) ;
#2746 = LINE ( 'NONE', #9583, #3167 ) ;
#2747 = CARTESIAN_POINT ( 'NONE',  ( -15.21174975910705207, 52.10286008774954780, 13.87500000000000000 ) ) ;
#2748 = FACE_OUTER_BOUND ( 'NONE', #931, .T. ) ;
#2749 = ORIENTED_EDGE ( 'NONE', *, *, #8772, .T. ) ;
#2750 = ADVANCED_FACE ( 'NONE', ( #16132 ), #6507, .T. ) ;
#2751 = VECTOR ( 'NONE', #18342, 1000.000000000000000 ) ;
#2752 = AXIS2_PLACEMENT_3D ( 'NONE', #20154, #9226, #5778 ) ;
#2753 = DIRECTION ( 'NONE',  ( -2.546383084002652634E-16, 0.000000000000000000, -1.000000000000000000 ) ) ;
#2754 = CIRCLE ( 'NONE', #15254, 0.2999999999999947153 ) ;
#2755 = VERTEX_POINT ( 'NONE', #12653 ) ;
#2756 = DIRECTION ( 'NONE',  ( -1.000000000000000000, 0.000000000000000000, 0.000000000000000000 ) ) ;
#2757 = VECTOR ( 'NONE', #10667, 1000.000000000000000 ) ;
#2758 = CARTESIAN_POINT ( 'NONE',  ( -23.02398829872514696, -2.279713943076945526, 13.43059441564925649 ) ) ;
#2759 = ORIENTED_EDGE ( 'NONE', *, *, #6572, .T. ) ;
#2760 = CIRCLE ( 'NONE', #4554, 0.05000000000000143219 ) ;
#2761 = ORIENTED_EDGE ( 'NONE', *, *, #9319, .F. ) ;
#2762 = CARTESIAN_POINT ( 'NONE',  ( -14.71432566477614579, 52.07267295633236870, 13.50000000000000000 ) ) ;
#2763 = CARTESIAN_POINT ( 'NONE',  ( -15.95292532278785913, 50.11873716947361856, 13.79999999999999893 ) ) ;
#2764 = EDGE_CURVE ( 'NONE', #11913, #3158, #10072, .T. ) ;
#2765 = CARTESIAN_POINT ( 'NONE',  ( -17.95292532278785913, 38.74634676501045760, 13.99999999999999822 ) ) ;
#2766 = EDGE_LOOP ( 'NONE', ( #19772, #18008, #137, #4940 ) ) ;
#2767 = ORIENTED_EDGE ( 'NONE', *, *, #21139, .T. ) ;
#2768 = CIRCLE ( 'NONE', #16699, 2.000000000000001776 ) ;
#2769 = DIRECTION ( 'NONE',  ( 0.000000000000000000, 0.000000000000000000, 1.000000000000000000 ) ) ;
#2770 = CIRCLE ( 'NONE', #21003, 0.05000000000000143219 ) ;
#2771 = TOROIDAL_SURFACE ( 'NONE', #12744, 0.2500000000000000000, 0.2500000000000000000 ) ;
#2772 = DIRECTION ( 'NONE',  ( -1.000000000000000000, 0.000000000000000000, 0.000000000000000000 ) ) ;
#2773 = FACE_OUTER_BOUND ( 'NONE', #16639, .T. ) ;
#2774 = DIRECTION ( 'NONE',  ( 0.000000000000000000, 1.000000000000000000, 0.000000000000000000 ) ) ;
#2775 = VECTOR ( 'NONE', #19857, 1000.000000000000000 ) ;
#2776 = DIRECTION ( 'NONE',  ( -0.000000000000000000, -0.000000000000000000, -1.000000000000000000 ) ) ;
#2777 = DIRECTION ( 'NONE',  ( 0.000000000000000000, 1.000000000000000000, -0.000000000000000000 ) ) ;
#2778 = CIRCLE ( 'NONE', #20287, 0.05000000000000143219 ) ;
#2779 = EDGE_CURVE ( 'NONE', #10550, #6305, #11839, .T. ) ;
#2780 = CARTESIAN_POINT ( 'NONE',  ( -29.50000000000001421, -69.00000000000000000, 0.1242640687119232062 ) ) ;
#2781 = ORIENTED_EDGE ( 'NONE', *, *, #13018, .F. ) ;
#2782 = DIRECTION ( 'NONE',  ( 1.734723475976806848E-16, 0.000000000000000000, -1.000000000000000000 ) ) ;
#2783 = CARTESIAN_POINT ( 'NONE',  ( 1.724728116533979616, 43.26054587065083012, 37.76679706732590347 ) ) ;
#2784 = CARTESIAN_POINT ( 'NONE',  ( -29.69597781366221767, 58.69165929845684815, 68.50000000000000000 ) ) ;
#2785 = AXIS2_PLACEMENT_3D ( 'NONE', #9123, #7573, #19316 ) ;
#2786 = AXIS2_PLACEMENT_3D ( 'NONE', #11897, #1603, #8568 ) ;
#2787 = AXIS2_PLACEMENT_3D ( 'NONE', #10728, #9147, #10502 ) ;
#2788 = ORIENTED_EDGE ( 'NONE', *, *, #20870, .T. ) ;
#2789 = DIRECTION ( 'NONE',  ( 0.000000000000000000, 0.000000000000000000, -1.000000000000000000 ) ) ;
#2790 = ADVANCED_FACE ( 'NONE', ( #19843 ), #16479, .T. ) ;
#2791 = EDGE_CURVE ( 'NONE', #16467, #14127, #21148, .T. ) ;
#2792 = CYLINDRICAL_SURFACE ( 'NONE', #14912, 0.1000000000000028644 ) ;
#2793 = ORIENTED_EDGE ( 'NONE', *, *, #8910, .F. ) ;
#2794 = EDGE_CURVE ( 'NONE', #19805, #620, #7653, .T. ) ;
#2795 = CIRCLE ( 'NONE', #12765, 0.2999999999999999334 ) ;
#2796 = ORIENTED_EDGE ( 'NONE', *, *, #21723, .F. ) ;
#2797 = AXIS2_PLACEMENT_3D ( 'NONE', #14005, #21082, #244 ) ;
#2798 = LINE ( 'NONE', #9397, #17452 ) ;
#2799 = CIRCLE ( 'NONE', #21033, 1.974596669241483804 ) ;
#2800 = ORIENTED_EDGE ( 'NONE', *, *, #3164, .F. ) ;
#2801 = DIRECTION ( 'NONE',  ( 1.000000000000000000, -0.000000000000000000, -0.000000000000000000 ) ) ;
#2802 = CARTESIAN_POINT ( 'NONE',  ( 0.000000000000000000, -51.61873716947361856, 68.00000000000000000 ) ) ;
#2803 = VECTOR ( 'NONE', #16472, 1000.000000000000000 ) ;
#2804 = CIRCLE ( 'NONE', #6403, 0.05000000000000143219 ) ;
#2805 = VERTEX_POINT ( 'NONE', #19620 ) ;
#2806 = CARTESIAN_POINT ( 'NONE',  ( 15.21174975910707161, 41.81054587065082728, 68.25000000000000000 ) ) ;
#2807 = FACE_OUTER_BOUND ( 'NONE', #1578, .T. ) ;
#2808 = EDGE_CURVE ( 'NONE', #20015, #6058, #16234, .T. ) ;
#2809 = CARTESIAN_POINT ( 'NONE',  ( -8.638906393579159015, 41.42245079618239600, 68.06527860057354928 ) ) ;
#2810 = AXIS2_PLACEMENT_3D ( 'NONE', #18188, #622, #4098 ) ;
#2811 = CIRCLE ( 'NONE', #3891, 1.999999999999991340 ) ;
#2812 = DIRECTION ( 'NONE',  ( 0.000000000000000000, 0.000000000000000000, -1.000000000000000000 ) ) ;
#2813 = AXIS2_PLACEMENT_3D ( 'NONE', #20719, #3819, #17461 ) ;
#2814 = DIRECTION ( 'NONE',  ( 0.000000000000000000, 1.000000000000000000, 0.000000000000000000 ) ) ;
#2815 = VECTOR ( 'NONE', #20240, 1000.000000000000000 ) ;
#2816 = CARTESIAN_POINT ( 'NONE',  ( 1.824728116533979261, 43.26054587065083012, 43.80876104995653719 ) ) ;
#2817 = DIRECTION ( 'NONE',  ( 1.000000000000000000, 0.000000000000000000, 0.000000000000000000 ) ) ;
#2818 = ADVANCED_FACE ( 'NONE', ( #13234 ), #4399, .F. ) ;
#2819 = VERTEX_POINT ( 'NONE', #1246 ) ;
#2820 = DIRECTION ( 'NONE',  ( 0.000000000000000000, 0.000000000000000000, 1.000000000000000000 ) ) ;
#2821 = ADVANCED_FACE ( 'NONE', ( #6316 ), #6098, .T. ) ;
#2822 = AXIS2_PLACEMENT_3D ( 'NONE', #12045, #15617, #16975 ) ;
#2823 = DIRECTION ( 'NONE',  ( 1.000000000000000000, 0.000000000000000000, 0.000000000000000000 ) ) ;
#2824 = ORIENTED_EDGE ( 'NONE', *, *, #7344, .F. ) ;
#2825 = ORIENTED_EDGE ( 'NONE', *, *, #3231, .T. ) ;
#2826 = DIRECTION ( 'NONE',  ( -1.000000000000000000, 0.000000000000000000, 0.000000000000000000 ) ) ;
#2827 = ADVANCED_FACE ( 'NONE', ( #21425 ), #2843, .F. ) ;
#2828 = CARTESIAN_POINT ( 'NONE',  ( 0.000000000000000000, 0.000000000000000000, 0.000000000000000000 ) ) ;
#2829 = DIRECTION ( 'NONE',  ( 0.000000000000000000, -1.000000000000000000, 0.000000000000000000 ) ) ;
#2830 = UNCERTAINTY_MEASURE_WITH_UNIT (LENGTH_MEASURE( 1.000000000000000082E-05 ), #18722, 'distance_accuracy_value', 'NONE');
#2831 = TOROIDAL_SURFACE ( 'NONE', #20707, 0.05000000000000000278, 0.05000000000000000278 ) ;
#2832 = ORIENTED_EDGE ( 'NONE', *, *, #21476, .F. ) ;
#2833 = VERTEX_POINT ( 'NONE', #8102 ) ;
#2834 = CIRCLE ( 'NONE', #1760, 0.05000000000000143219 ) ;
#2835 = ORIENTED_EDGE ( 'NONE', *, *, #17544, .T. ) ;
#2836 = ORIENTED_EDGE ( 'NONE', *, *, #13992, .F. ) ;
#2837 = EDGE_CURVE ( 'NONE', #10741, #6249, #7938, .T. ) ;
#2838 = CARTESIAN_POINT ( 'NONE',  ( 15.06741964789885024, -51.94542257242142824, 13.49999999999999645 ) ) ;
#2839 = DIRECTION ( 'NONE',  ( 0.000000000000000000, 0.000000000000000000, 1.000000000000000000 ) ) ;
#2840 = ORIENTED_EDGE ( 'NONE', *, *, #21774, .F. ) ;
#2841 = LINE ( 'NONE', #16233, #7885 ) ;
#2842 = ADVANCED_FACE ( 'NONE', ( #2714 ), #16890, .F. ) ;
#2843 = CYLINDRICAL_SURFACE ( 'NONE', #20442, 0.3000000000000016542 ) ;
#2844 = AXIS2_PLACEMENT_3D ( 'NONE', #3025, #5770, #10790 ) ;
#2845 = DIRECTION ( 'NONE',  ( 1.000000000000000000, 0.000000000000000000, 0.000000000000000000 ) ) ;
#2846 = DIRECTION ( 'NONE',  ( -1.000000000000000000, 0.000000000000000000, -1.987703982890080681E-15 ) ) ;
#2847 = EDGE_LOOP ( 'NONE', ( #16270, #4302, #21018, #2695 ) ) ;
#2848 = DIRECTION ( 'NONE',  ( -0.000000000000000000, -0.000000000000000000, -1.000000000000000000 ) ) ;
#2849 = ORIENTED_EDGE ( 'NONE', *, *, #21144, .F. ) ;
#2850 = ORIENTED_EDGE ( 'NONE', *, *, #12933, .T. ) ;
#2851 = VERTEX_POINT ( 'NONE', #7990 ) ;
#2852 = DIRECTION ( 'NONE',  ( 0.000000000000000000, 0.000000000000000000, 1.000000000000000000 ) ) ;
#2853 = EDGE_CURVE ( 'NONE', #2179, #22131, #8681, .T. ) ;
#2854 = CARTESIAN_POINT ( 'NONE',  ( -1.774728116533986766, 42.36054587065083155, 37.66679706732590915 ) ) ;
#2855 = ORIENTED_EDGE ( 'NONE', *, *, #3962, .F. ) ;
#2856 = AXIS2_PLACEMENT_3D ( 'NONE', #4295, #16235, #19622 ) ;
#2857 = FACE_OUTER_BOUND ( 'NONE', #12159, .T. ) ;
#2858 = VECTOR ( 'NONE', #11537, 1000.000000000000000 ) ;
#2859 = TOROIDAL_SURFACE ( 'NONE', #16428, 1.000000000000000000, 0.5000000000000000000 ) ;
#2860 = ORIENTED_EDGE ( 'NONE', *, *, #5270, .F. ) ;
#2861 = FACE_OUTER_BOUND ( 'NONE', #5265, .T. ) ;
#2862 = DIRECTION ( 'NONE',  ( -0.000000000000000000, -1.000000000000000000, -0.000000000000000000 ) ) ;
#2863 = CARTESIAN_POINT ( 'NONE',  ( 30.79999999999999716, -85.00000000000000000, 0.3000000000000039857 ) ) ;
#2864 = CARTESIAN_POINT ( 'NONE',  ( 23.02398829872513986, 2.157133568460765538, 13.19999999999999929 ) ) ;
#2865 = FACE_OUTER_BOUND ( 'NONE', #7165, .T. ) ;
#2866 = EDGE_LOOP ( 'NONE', ( #10903, #19261, #10500, #14904 ) ) ;
#2867 = CARTESIAN_POINT ( 'NONE',  ( -3.627054932750481964, -33.93424481021354921, 68.50000000000000000 ) ) ;
#2868 = CARTESIAN_POINT ( 'NONE',  ( 30.79999999999999716, -123.9599366953518711, 1.200000000000003064 ) ) ;
#2869 = EDGE_CURVE ( 'NONE', #2394, #19800, #5830, .T. ) ;
#2870 = CARTESIAN_POINT ( 'NONE',  ( -23.61959064016851073, 45.26242829375641463, 68.25000000000000000 ) ) ;
#2871 = EDGE_CURVE ( 'NONE', #20113, #11406, #98, .T. ) ;
#2872 = CARTESIAN_POINT ( 'NONE',  ( -1.724728116533986721, 42.31054587065082728, 33.66679706732590915 ) ) ;
#2873 = CARTESIAN_POINT ( 'NONE',  ( -23.02398829872513986, 7.027230193580998154E-15, 13.79999999999999893 ) ) ;
#2874 = ORIENTED_EDGE ( 'NONE', *, *, #8795, .F. ) ;
#2875 = ADVANCED_FACE ( 'NONE', ( #18373 ), #12223, .T. ) ;
#2876 = CYLINDRICAL_SURFACE ( 'NONE', #14111, 0.3000000000000016542 ) ;
#2877 = CARTESIAN_POINT ( 'NONE',  ( -1.824728116533986810, 43.31054587065082728, 37.76679706732590347 ) ) ;
#2878 = CIRCLE ( 'NONE', #15731, 0.2999999999999947153 ) ;
#2879 = ORIENTED_EDGE ( 'NONE', *, *, #19114, .F. ) ;
#2880 = VECTOR ( 'NONE', #12883, 1000.000000000000000 ) ;
#2881 = LINE ( 'NONE', #14824, #17678 ) ;
#2882 = CARTESIAN_POINT ( 'NONE',  ( 8.641460742840918030, 33.43424481021354921, 68.50000000000000000 ) ) ;
#2883 = ORIENTED_EDGE ( 'NONE', *, *, #11039, .T. ) ;
#2884 = EDGE_LOOP ( 'NONE', ( #21358, #4109, #16987, #7689 ) ) ;
#2885 = EDGE_LOOP ( 'NONE', ( #566, #4696, #15517, #3939 ) ) ;
#2886 = DIRECTION ( 'NONE',  ( 0.000000000000000000, 0.000000000000000000, 1.000000000000000000 ) ) ;
#2887 = CARTESIAN_POINT ( 'NONE',  ( 1.724728116533979616, 42.31054587065082728, 27.75876104995653648 ) ) ;
#2888 = FACE_OUTER_BOUND ( 'NONE', #568, .T. ) ;
#2889 = ORIENTED_EDGE ( 'NONE', *, *, #5928, .F. ) ;
#2890 = VERTEX_POINT ( 'NONE', #18271 ) ;
#2891 = PRODUCT_DEFINITION ( 'UNKNOWN', '', #18732, #13558 ) ;
#2892 = CARTESIAN_POINT ( 'NONE',  ( 29.50000000000002132, 69.00000000000000000, 0.2999999999999947153 ) ) ;
#2893 = AXIS2_PLACEMENT_3D ( 'NONE', #16101, #7628, #6068 ) ;
#2894 = FACE_OUTER_BOUND ( 'NONE', #2909, .T. ) ;
#2895 = CARTESIAN_POINT ( 'NONE',  ( -23.02398829872513986, -2.681050038336388663, 13.50121499737458564 ) ) ;
#2896 = CIRCLE ( 'NONE', #15732, 0.05000000000000143219 ) ;
#2897 = CARTESIAN_POINT ( 'NONE',  ( 1.724728116533979838, 42.36054587065083155, 41.66679706732590915 ) ) ;
#2898 = CARTESIAN_POINT ( 'NONE',  ( -23.75488095381848197, 42.46645089659918426, 68.25000000000000000 ) ) ;
#2899 = CARTESIAN_POINT ( 'NONE',  ( -9.978973617317260292, 41.92645089659918511, 68.06527860057354928 ) ) ;
#2900 = DIRECTION ( 'NONE',  ( -2.107255972849994642E-16, 0.000000000000000000, -1.000000000000000000 ) ) ;
#2901 = EDGE_CURVE ( 'NONE', #1780, #20330, #810, .T. ) ;
#2902 = EDGE_LOOP ( 'NONE', ( #11148, #3601, #20243, #1179 ) ) ;
#2903 = ADVANCED_FACE ( 'NONE', ( #21308 ), #18488, .F. ) ;
#2904 = FACE_OUTER_BOUND ( 'NONE', #14726, .T. ) ;
#2905 = CARTESIAN_POINT ( 'NONE',  ( -1.724728116533986721, 43.26054587065083012, 39.75876104995654003 ) ) ;
#2906 = LINE ( 'NONE', #8167, #17228 ) ;
#2907 = ORIENTED_EDGE ( 'NONE', *, *, #18261, .F. ) ;
#2908 = DIRECTION ( 'NONE',  ( 3.543406725251269872E-15, -1.000000000000000000, -5.100473277356134011E-17 ) ) ;
#2909 = EDGE_LOOP ( 'NONE', ( #3326, #19451, #17481, #12974 ) ) ;
#2910 = ORIENTED_EDGE ( 'NONE', *, *, #21503, .T. ) ;
#2911 = CARTESIAN_POINT ( 'NONE',  ( -1.824728116533986810, 42.36054587065083155, 35.80876104995653009 ) ) ;
#2912 = ORIENTED_EDGE ( 'NONE', *, *, #20121, .F. ) ;
#2913 = AXIS2_PLACEMENT_3D ( 'NONE', #20867, #5440, #12227 ) ;
#2914 = LINE ( 'NONE', #4370, #780 ) ;
#2915 = VERTEX_POINT ( 'NONE', #15125 ) ;
#2916 = CARTESIAN_POINT ( 'NONE',  ( -23.02398829872514341, -5.683640910026986681, 13.79999999999999893 ) ) ;
#2917 = AXIS2_PLACEMENT_3D ( 'NONE', #3747, #3541, #10569 ) ;
#2918 = EDGE_CURVE ( 'NONE', #20326, #5502, #17145, .T. ) ;
#2919 = DIRECTION ( 'NONE',  ( -1.000000000000000000, 0.000000000000000000, 0.000000000000000000 ) ) ;
#2920 = FACE_OUTER_BOUND ( 'NONE', #5704, .T. ) ;
#2921 = DIRECTION ( 'NONE',  ( -0.000000000000000000, 1.000000000000000000, -0.000000000000000000 ) ) ;
#2922 = DIRECTION ( 'NONE',  ( 0.000000000000000000, 0.000000000000000000, 1.000000000000000000 ) ) ;
#2923 = CARTESIAN_POINT ( 'NONE',  ( 17.92752199202934094, 50.11873716947361856, 13.79999999999999893 ) ) ;
#2924 = LINE ( 'NONE', #4271, #10158 ) ;
#2925 = CARTESIAN_POINT ( 'NONE',  ( 31.63662752439705272, 0.000000000000000000, -18.50000000000000000 ) ) ;
#2926 = CARTESIAN_POINT ( 'NONE',  ( 28.87540678000427263, -6.494748934539262386, 7.720760203330568672 ) ) ;
#2927 = ORIENTED_EDGE ( 'NONE', *, *, #15789, .T. ) ;
#2928 = VECTOR ( 'NONE', #12425, 1000.000000000000000 ) ;
#2929 = CARTESIAN_POINT ( 'NONE',  ( 32.20000000000001705, 0.000000000000000000, 3.200000000000000178 ) ) ;
#2930 = VERTEX_POINT ( 'NONE', #10337 ) ;
#2931 = DIRECTION ( 'NONE',  ( -0.000000000000000000, 1.000000000000000000, -0.000000000000000000 ) ) ;
#2932 = VECTOR ( 'NONE', #13852, 1000.000000000000000 ) ;
#2933 = CARTESIAN_POINT ( 'NONE',  ( -35.00000000000000000, -84.70000000000001705, 0.2999999999999999889 ) ) ;
#2934 = EDGE_LOOP ( 'NONE', ( #13699, #7776, #8142, #5644 ) ) ;
#2935 = EDGE_LOOP ( 'NONE', ( #12583, #7081, #8810, #14553 ) ) ;
#2936 = LINE ( 'NONE', #4492, #18148 ) ;
#2937 = SURFACE_STYLE_FILL_AREA ( #12980 ) ;
#2938 = ADVANCED_FACE ( 'NONE', ( #5075 ), #19756, .F. ) ;
#2939 =( NAMED_UNIT ( * ) PLANE_ANGLE_UNIT ( ) SI_UNIT ( $, .RADIAN. ) );
#2940 = EDGE_LOOP ( 'NONE', ( #8384, #1084, #8140, #19016 ) ) ;
#2941 = VERTEX_POINT ( 'NONE', #13449 ) ;
#2942 = ORIENTED_EDGE ( 'NONE', *, *, #21673, .T. ) ;
#2943 = EDGE_CURVE ( 'NONE', #4058, #14043, #16695, .T. ) ;
#2944 = AXIS2_PLACEMENT_3D ( 'NONE', #3361, #21950, #6742 ) ;
#2945 = EDGE_CURVE ( 'NONE', #16071, #15168, #18712, .T. ) ;
#2946 = DIRECTION ( 'NONE',  ( 1.000000000000000000, 0.000000000000000000, 0.000000000000000000 ) ) ;
#2947 = VECTOR ( 'NONE', #4027, 1000.000000000000000 ) ;
#2948 = EDGE_CURVE ( 'NONE', #852, #15775, #11520, .T. ) ;
#2949 = DIRECTION ( 'NONE',  ( 1.224646799147353207E-16, 0.000000000000000000, 1.000000000000000000 ) ) ;
#2950 = EDGE_LOOP ( 'NONE', ( #7873, #20500, #10760, #2671 ) ) ;
#2951 = EDGE_CURVE ( 'NONE', #15636, #5056, #20289, .T. ) ;
#2952 = DIRECTION ( 'NONE',  ( -1.000000000000000000, 0.000000000000000000, 0.000000000000000000 ) ) ;
#2953 = DIRECTION ( 'NONE',  ( 0.000000000000000000, 0.000000000000000000, 1.000000000000000000 ) ) ;
#2954 = CYLINDRICAL_SURFACE ( 'NONE', #5235, 0.3000000000000003775 ) ;
#2955 = LINE ( 'NONE', #3390, #16493 ) ;
#2956 = ORIENTED_EDGE ( 'NONE', *, *, #17439, .F. ) ;
#2957 = EDGE_LOOP ( 'NONE', ( #20095, #16910, #376, #14085 ) ) ;
#2958 = ORIENTED_EDGE ( 'NONE', *, *, #10719, .F. ) ;
#2959 = DIRECTION ( 'NONE',  ( 0.000000000000000000, 0.000000000000000000, 1.000000000000000000 ) ) ;
#2960 = CARTESIAN_POINT ( 'NONE',  ( 25.37540678000426908, 36.74634676501047181, 42.50000000000000000 ) ) ;
#2961 = EDGE_CURVE ( 'NONE', #170, #13966, #5482, .T. ) ;
#2962 = ORIENTED_EDGE ( 'NONE', *, *, #2506, .T. ) ;
#2963 = CARTESIAN_POINT ( 'NONE',  ( 25.37540678000427263, 68.44634676501046044, 7.500000000000000000 ) ) ;
#2964 = ORIENTED_EDGE ( 'NONE', *, *, #4035, .T. ) ;
#2965 = DIRECTION ( 'NONE',  ( 1.224646799147353207E-16, 0.000000000000000000, 1.000000000000000000 ) ) ;
#2966 = CARTESIAN_POINT ( 'NONE',  ( -9.141460742840918030, 33.43424481021354921, 68.00000000000000000 ) ) ;
#2967 = DIRECTION ( 'NONE',  ( -0.000000000000000000, -0.000000000000000000, -1.000000000000000000 ) ) ;
#2968 = EDGE_CURVE ( 'NONE', #14823, #4085, #3681, .T. ) ;
#2969 = CARTESIAN_POINT ( 'NONE',  ( -30.79999999999999005, 69.70000000000001705, 1.200000000000000400 ) ) ;
#2970 = VERTEX_POINT ( 'NONE', #12100 ) ;
#2971 = CARTESIAN_POINT ( 'NONE',  ( -15.95292532278785913, -50.11873716947361856, 13.79999999999999893 ) ) ;
#2972 = EDGE_CURVE ( 'NONE', #8448, #6694, #9999, .T. ) ;
#2973 = CYLINDRICAL_SURFACE ( 'NONE', #7494, 0.2999999999999999334 ) ;
#2974 = DIRECTION ( 'NONE',  ( -1.000000000000000000, 0.000000000000000000, 0.000000000000000000 ) ) ;
#2975 = CARTESIAN_POINT ( 'NONE',  ( -11.62890639357915923, 41.92645089659917801, 70.88527860057354246 ) ) ;
#2976 = ORIENTED_EDGE ( 'NONE', *, *, #1124, .F. ) ;
#2977 = DIRECTION ( 'NONE',  ( 0.000000000000000000, 0.000000000000000000, 1.000000000000000000 ) ) ;
#2978 = CARTESIAN_POINT ( 'NONE',  ( -31.50000000000002132, -71.00000000000001421, 1.500000000000000000 ) ) ;
#2979 = DIRECTION ( 'NONE',  ( 0.000000000000000000, 0.000000000000000000, -1.000000000000000000 ) ) ;
#2980 = EDGE_LOOP ( 'NONE', ( #13397, #22070, #7365, #9979 ) ) ;
#2981 = CARTESIAN_POINT ( 'NONE',  ( 1.774728116533979883, 43.26054587065083012, 41.66679706732590915 ) ) ;
#2982 = CYLINDRICAL_SURFACE ( 'NONE', #933, 0.2999999999999999334 ) ;
#2983 = ORIENTED_EDGE ( 'NONE', *, *, #17401, .F. ) ;
#2984 = ORIENTED_EDGE ( 'NONE', *, *, #6116, .T. ) ;
#2985 = ORIENTED_EDGE ( 'NONE', *, *, #13357, .F. ) ;
#2986 = CARTESIAN_POINT ( 'NONE',  ( -29.50000000000001421, 69.00000000000000000, 0.1242640687119232062 ) ) ;
#2987 = DIRECTION ( 'NONE',  ( 1.000000000000000000, 0.000000000000000000, 0.000000000000000000 ) ) ;
#2988 = PRESENTATION_LAYER_ASSIGNMENT (  '', '', ( #9778 ) ) ;
#2989 = ORIENTED_EDGE ( 'NONE', *, *, #10202, .T. ) ;
#2990 = EDGE_CURVE ( 'NONE', #15493, #416, #8324, .T. ) ;
#2991 = EDGE_CURVE ( 'NONE', #8252, #897, #11167, .T. ) ;
#2992 = EDGE_LOOP ( 'NONE', ( #2283, #15480, #16801, #15062 ) ) ;
#2993 = LINE ( 'NONE', #7935, #12879 ) ;
#2994 = DIRECTION ( 'NONE',  ( 0.000000000000000000, 0.000000000000000000, 1.000000000000000000 ) ) ;
#2995 = CARTESIAN_POINT ( 'NONE',  ( -23.02398829872514341, -2.558844643945016539, 13.47100117844888700 ) ) ;
#2996 = CARTESIAN_POINT ( 'NONE',  ( 15.21174975910705918, 51.61873716947361856, 14.00000000000000000 ) ) ;
#2997 = DIRECTION ( 'NONE',  ( 0.000000000000000000, 0.000000000000000000, 1.000000000000000000 ) ) ;
#2998 = DIRECTION ( 'NONE',  ( -0.000000000000000000, -1.000000000000000000, -0.000000000000000000 ) ) ;
#2999 = EDGE_CURVE ( 'NONE', #11094, #18906, #11771, .T. ) ;
#3000 = CARTESIAN_POINT ( 'NONE',  ( 15.21174975910707161, 41.81054587065082728, 68.50000000000000000 ) ) ;
#3001 = DIRECTION ( 'NONE',  ( 1.000000000000000000, 0.000000000000000000, 0.000000000000000000 ) ) ;
#3002 = FACE_OUTER_BOUND ( 'NONE', #7067, .T. ) ;
#3003 = AXIS2_PLACEMENT_3D ( 'NONE', #6752, #12085, #336 ) ;
#3004 = ORIENTED_EDGE ( 'NONE', *, *, #7645, .F. ) ;
#3005 = CARTESIAN_POINT ( 'NONE',  ( -21.92816239687475743, 42.46645089659918426, 13.50000000000000000 ) ) ;
#3006 = DIRECTION ( 'NONE',  ( 1.000000000000000000, 0.000000000000000000, 0.000000000000000000 ) ) ;
#3007 = DIRECTION ( 'NONE',  ( 0.000000000000000000, 0.000000000000000000, 1.000000000000000000 ) ) ;
#3008 = ORIENTED_EDGE ( 'NONE', *, *, #18971, .T. ) ;
#3009 = DIRECTION ( 'NONE',  ( 0.000000000000000000, 0.000000000000000000, 1.000000000000000000 ) ) ;
#3011 = CIRCLE ( 'NONE', #18725, 0.04999999999999991257 ) ;
#3010 = DIRECTION ( 'NONE',  ( 0.000000000000000000, -1.000000000000000000, 0.000000000000000000 ) ) ;
#3012 = EDGE_LOOP ( 'NONE', ( #11795, #6549, #6913, #21826 ) ) ;
#3013 = VERTEX_POINT ( 'NONE', #11983 ) ;
#3014 = CARTESIAN_POINT ( 'NONE',  ( 29.33570557543480462, -2.657597333499439607, 0.02220207281669739699 ) ) ;
#3015 = ADVANCED_FACE ( 'NONE', ( #20626 ), #2267, .F. ) ;
#3016 = ORIENTED_EDGE ( 'NONE', *, *, #2564, .F. ) ;
#3017 = EDGE_CURVE ( 'NONE', #4254, #18602, #7265, .T. ) ;
#3018 = CIRCLE ( 'NONE', #8375, 0.5000000000000000000 ) ;
#3019 = LINE ( 'NONE', #4808, #18860 ) ;
#3020 = ORIENTED_EDGE ( 'NONE', *, *, #2273, .T. ) ;
#3021 = DIRECTION ( 'NONE',  ( 0.000000000000000000, 0.000000000000000000, -1.000000000000000000 ) ) ;
#3022 = DIRECTION ( 'NONE',  ( -0.000000000000000000, -0.000000000000000000, -1.000000000000000000 ) ) ;
#3023 = DIRECTION ( 'NONE',  ( -2.546383084002652634E-16, 0.000000000000000000, -1.000000000000000000 ) ) ;
#3024 = FACE_OUTER_BOUND ( 'NONE', #9239, .T. ) ;
#3025 = CARTESIAN_POINT ( 'NONE',  ( -30.67540678000427690, 6.000000000000000000, 3.799999999999999822 ) ) ;
#3026 = CYLINDRICAL_SURFACE ( 'NONE', #5409, 0.5000000000000004441 ) ;
#3027 = CARTESIAN_POINT ( 'NONE',  ( 1.724728116533979616, 42.36054587065083155, 35.80876104995653009 ) ) ;
#3028 = CARTESIAN_POINT ( 'NONE',  ( -31.69597781366221412, 27.99124249474150972, 70.50000000000000000 ) ) ;
#3030 = EDGE_CURVE ( 'NONE', #17645, #15161, #12200, .T. ) ;
#3029 = DIRECTION ( 'NONE',  ( -1.000000000000000000, -0.000000000000000000, 0.000000000000000000 ) ) ;
#3031 = TOROIDAL_SURFACE ( 'NONE', #1599, 0.05000000000000000278, 0.05000000000000000278 ) ;
#3032 = EDGE_LOOP ( 'NONE', ( #14421, #13611, #11886, #3065 ) ) ;
#3033 = CARTESIAN_POINT ( 'NONE',  ( 1.724728116533979616, 43.26054587065083012, 31.70876104995653932 ) ) ;
#3034 = ORIENTED_EDGE ( 'NONE', *, *, #996, .T. ) ;
#3035 = DIRECTION ( 'NONE',  ( 1.000000000000000000, 0.000000000000000000, 0.000000000000000000 ) ) ;
#3036 = CYLINDRICAL_SURFACE ( 'NONE', #4222, 2.000000000000000000 ) ;
#3037 = ORIENTED_EDGE ( 'NONE', *, *, #5928, .T. ) ;
#3038 = ORIENTED_EDGE ( 'NONE', *, *, #20316, .F. ) ;
#3039 = CARTESIAN_POINT ( 'NONE',  ( -3.627054932750481964, -33.43424481021354921, 7.321391277662001151 ) ) ;
#3040 = EDGE_CURVE ( 'NONE', #14913, #8265, #17953, .T. ) ;
#3041 =( NAMED_UNIT ( * ) PLANE_ANGLE_UNIT ( ) SI_UNIT ( $, .RADIAN. ) );
#3042 = ORIENTED_EDGE ( 'NONE', *, *, #11291, .T. ) ;
#3043 = ORIENTED_EDGE ( 'NONE', *, *, #11546, .T. ) ;
#3044 = ORIENTED_EDGE ( 'NONE', *, *, #14343, .F. ) ;
#3045 = CIRCLE ( 'NONE', #19472, 3.500000000000003109 ) ;
#3046 = ORIENTED_EDGE ( 'NONE', *, *, #9096, .F. ) ;
#3047 = CYLINDRICAL_SURFACE ( 'NONE', #12741, 0.2999999999999999334 ) ;
#3048 = DIRECTION ( 'NONE',  ( 0.000000000000000000, 0.000000000000000000, 1.000000000000000000 ) ) ;
#3049 = ORIENTED_EDGE ( 'NONE', *, *, #16563, .F. ) ;
#3050 = CARTESIAN_POINT ( 'NONE',  ( 8.641460742840918030, -33.43424481021354921, 42.50000000000000000 ) ) ;
#3051 = ADVANCED_FACE ( 'NONE', ( #19477 ), #3718, .F. ) ;
#3052 = DIRECTION ( 'NONE',  ( 1.000000000000000000, -0.000000000000000000, 0.000000000000000000 ) ) ;
#3053 = VECTOR ( 'NONE', #3022, 1000.000000000000000 ) ;
#3054 = CARTESIAN_POINT ( 'NONE',  ( -1.724728116533986721, 43.31054587065082728, 49.76679706732591058 ) ) ;
#3055 = ORIENTED_EDGE ( 'NONE', *, *, #10613, .F. ) ;
#3056 = TOROIDAL_SURFACE ( 'NONE', #1615, 1.500000000000000000, 0.5000000000000000000 ) ;
#3057 = VERTEX_POINT ( 'NONE', #8872 ) ;
#3058 = CIRCLE ( 'NONE', #16259, 0.05000000000000143219 ) ;
#3059 = CIRCLE ( 'NONE', #905, 0.05000000000000143219 ) ;
#3060 = EDGE_LOOP ( 'NONE', ( #3393, #5780, #14038, #161, #18929, #3020 ) ) ;
#3061 = DIRECTION ( 'NONE',  ( 0.000000000000000000, 0.000000000000000000, -1.000000000000000000 ) ) ;
#3062 = ADVANCED_FACE ( 'NONE', ( #351 ), #7198, .F. ) ;
#3063 = DIRECTION ( 'NONE',  ( 0.000000000000000000, 0.000000000000000000, 1.000000000000000000 ) ) ;
#3064 = EDGE_CURVE ( 'NONE', #5550, #14977, #4748, .T. ) ;
#3065 = ORIENTED_EDGE ( 'NONE', *, *, #19169, .F. ) ;
#3066 = EDGE_CURVE ( 'NONE', #12192, #799, #21912, .T. ) ;
#3067 = DIRECTION ( 'NONE',  ( -1.000000000000000000, 0.000000000000000000, 1.224646799147353207E-16 ) ) ;
#3068 = EDGE_LOOP ( 'NONE', ( #13296, #8856, #11876, #10419 ) ) ;
#3069 = DIRECTION ( 'NONE',  ( 0.000000000000000000, 1.000000000000000000, 0.000000000000000000 ) ) ;
#3070 = DIRECTION ( 'NONE',  ( 0.000000000000000000, -1.000000000000000000, 0.000000000000000000 ) ) ;
#3071 = DIRECTION ( 'NONE',  ( 0.000000000000000000, 1.000000000000000000, 0.000000000000000000 ) ) ;
#3072 = VECTOR ( 'NONE', #7659, 1000.000000000000000 ) ;
#3073 = CARTESIAN_POINT ( 'NONE',  ( -15.21174975910705207, -51.61873716947361856, 68.50000000000000000 ) ) ;
#3074 = TOROIDAL_SURFACE ( 'NONE', #7733, 0.05000000000000000278, 0.05000000000000000278 ) ;
#3075 = ORIENTED_EDGE ( 'NONE', *, *, #19116, .F. ) ;
#3076 = DIRECTION ( 'NONE',  ( -1.000000000000000000, 0.000000000000000000, 0.000000000000000000 ) ) ;
#3077 = CARTESIAN_POINT ( 'NONE',  ( -15.21174975910705207, 41.81054587065082728, 13.75000000000000000 ) ) ;
#3078 = EDGE_CURVE ( 'NONE', #808, #1813, #16914, .T. ) ;
#3079 = CARTESIAN_POINT ( 'NONE',  ( -1.774728116533986766, 42.36054587065083155, 35.80876104995653009 ) ) ;
#3080 = VERTEX_POINT ( 'NONE', #7416 ) ;
#3081 = CARTESIAN_POINT ( 'NONE',  ( -20.10144383993102934, 42.46645089659918426, 13.74999999999999822 ) ) ;
#3082 = VERTEX_POINT ( 'NONE', #7533 ) ;
#3083 = DIRECTION ( 'NONE',  ( 5.192538640813645496E-17, -1.000000000000000000, -6.359025825921378559E-33 ) ) ;
#3084 = DIRECTION ( 'NONE',  ( 0.000000000000000000, 0.000000000000000000, 1.000000000000000000 ) ) ;
#3085 = ORIENTED_EDGE ( 'NONE', *, *, #9291, .T. ) ;
#3086 = AXIS2_PLACEMENT_3D ( 'NONE', #12296, #7409, #9080 ) ;
#3087 = VECTOR ( 'NONE', #7688, 1000.000000000000000 ) ;
#3088 = ORIENTED_EDGE ( 'NONE', *, *, #17186, .F. ) ;
#3089 = AXIS2_PLACEMENT_3D ( 'NONE', #2996, #9938, #9824 ) ;
#3090 = EDGE_LOOP ( 'NONE', ( #15141, #7206, #22045, #12292 ) ) ;
#3091 = CARTESIAN_POINT ( 'NONE',  ( -15.21174975910705385, 52.00603550409435627, 13.50000000000000000 ) ) ;
#3092 = EDGE_CURVE ( 'NONE', #5901, #13985, #5753, .T. ) ;
#3093 = DIRECTION ( 'NONE',  ( 0.000000000000000000, 0.000000000000000000, 1.000000000000000000 ) ) ;
#3094 = ADVANCED_FACE ( 'NONE', ( #4051 ), #21185, .F. ) ;
#3095 = ORIENTED_EDGE ( 'NONE', *, *, #473, .F. ) ;
#3096 = CIRCLE ( 'NONE', #2013, 2.767785046117004377 ) ;
#3097 = EDGE_CURVE ( 'NONE', #1750, #9565, #21734, .T. ) ;
#3098 = ORIENTED_EDGE ( 'NONE', *, *, #8129, .T. ) ;
#3099 = VERTEX_POINT ( 'NONE', #16551 ) ;
#3100 = DIRECTION ( 'NONE',  ( 0.000000000000000000, 0.000000000000000000, 1.000000000000000000 ) ) ;
#3101 = DIRECTION ( 'NONE',  ( -1.000000000000000000, 0.000000000000000000, 0.000000000000000000 ) ) ;
#3102 = CARTESIAN_POINT ( 'NONE',  ( -1.774728116533986766, 43.31054587065082728, 29.66679706732590560 ) ) ;
#3103 = FACE_OUTER_BOUND ( 'NONE', #18280, .T. ) ;
#3104 = AXIS2_PLACEMENT_3D ( 'NONE', #6457, #9572, #6224 ) ;
#3105 = CIRCLE ( 'NONE', #12137, 1.826718556943725202 ) ;
#3106 = TOROIDAL_SURFACE ( 'NONE', #10975, 2.274596669241483848, 0.2999999999999999889 ) ;
#3107 = DIRECTION ( 'NONE',  ( -1.000000000000000000, 0.000000000000000000, 0.000000000000000000 ) ) ;
#3108 = DIRECTION ( 'NONE',  ( 0.000000000000000000, -1.000000000000000000, 0.000000000000000000 ) ) ;
#3109 = ORIENTED_EDGE ( 'NONE', *, *, #5282, .T. ) ;
#3110 = CARTESIAN_POINT ( 'NONE',  ( -7.347880794884131322E-17, -85.00000000000000000, 1.200000000000002176 ) ) ;
#3111 = CIRCLE ( 'NONE', #8487, 4.700000000000002842 ) ;
#3112 = ADVANCED_FACE ( 'NONE', ( #14770 ), #6075, .T. ) ;
#3113 = DIRECTION ( 'NONE',  ( -1.000000000000000000, 0.000000000000000000, 0.000000000000000000 ) ) ;
#3114 = DIRECTION ( 'NONE',  ( 6.123233995736764803E-17, 0.000000000000000000, -1.000000000000000000 ) ) ;
#3115 = ORIENTED_EDGE ( 'NONE', *, *, #15221, .T. ) ;
#3116 = CARTESIAN_POINT ( 'NONE',  ( -0.000000000000000000, 51.61873716947361856, 68.50000000000000000 ) ) ;
#3117 = CIRCLE ( 'NONE', #20630, 0.2500000000000002220 ) ;
#3118 = ADVANCED_FACE ( 'NONE', ( #1219 ), #11418, .T. ) ;
#3119 = DIRECTION ( 'NONE',  ( -1.000000000000000000, -0.000000000000000000, -0.000000000000000000 ) ) ;
#3120 = ORIENTED_EDGE ( 'NONE', *, *, #9391, .F. ) ;
#3121 = CARTESIAN_POINT ( 'NONE',  ( 34.39999999999998437, 85.00000000000000000, 79.70000000000000284 ) ) ;
#3122 = DIRECTION ( 'NONE',  ( 0.000000000000000000, 0.000000000000000000, 1.000000000000000000 ) ) ;
#3123 = EDGE_LOOP ( 'NONE', ( #21386, #5828, #8706, #19486 ) ) ;
#3124 = VECTOR ( 'NONE', #16804, 1000.000000000000114 ) ;
#3125 = AXIS2_PLACEMENT_3D ( 'NONE', #7723, #14523, #19694 ) ;
#3126 = AXIS2_PLACEMENT_3D ( 'NONE', #3812, #9286, #19034 ) ;
#3127 = VERTEX_POINT ( 'NONE', #6412 ) ;
#3128 = FACE_OUTER_BOUND ( 'NONE', #332, .T. ) ;
#3129 = EDGE_CURVE ( 'NONE', #8243, #22, #9752, .T. ) ;
#3130 = AXIS2_PLACEMENT_3D ( 'NONE', #4782, #13705, #8701 ) ;
#3131 = CIRCLE ( 'NONE', #12075, 2.500000000000002220 ) ;
#3132 = AXIS2_PLACEMENT_3D ( 'NONE', #5910, #6141, #10931 ) ;
#3133 = DIRECTION ( 'NONE',  ( 0.000000000000000000, 0.000000000000000000, 1.000000000000000000 ) ) ;
#3134 = DIRECTION ( 'NONE',  ( 6.123233995736764803E-17, -0.000000000000000000, -1.000000000000000000 ) ) ;
#3135 = DIRECTION ( 'NONE',  ( -0.000000000000000000, -1.000000000000000000, -0.000000000000000000 ) ) ;
#3136 = CYLINDRICAL_SURFACE ( 'NONE', #15924, 0.04999999999999991257 ) ;
#3137 = AXIS2_PLACEMENT_3D ( 'NONE', #13305, #5146, #11950 ) ;
#3138 = VECTOR ( 'NONE', #19239, 1000.000000000000000 ) ;
#3139 = CIRCLE ( 'NONE', #18496, 4.193574995607837863 ) ;
#3140 = DIRECTION ( 'NONE',  ( 1.000000000000000000, 0.000000000000000000, 0.000000000000000000 ) ) ;
#3141 = CARTESIAN_POINT ( 'NONE',  ( 15.95292532278785913, 50.11873716947361856, 13.87499999999999822 ) ) ;
#3142 = ADVANCED_FACE ( 'NONE', ( #14428 ), #2591, .T. ) ;
#3143 = CARTESIAN_POINT ( 'NONE',  ( 23.02398829872513986, 2.157133568460765538, 42.50000000000000000 ) ) ;
#3144 = VECTOR ( 'NONE', #20147, 1000.000000000000000 ) ;
#3145 = DIRECTION ( 'NONE',  ( 0.000000000000000000, 0.000000000000000000, 1.000000000000000000 ) ) ;
#3146 = EDGE_CURVE ( 'NONE', #17988, #689, #19599, .T. ) ;
#3147 = CARTESIAN_POINT ( 'NONE',  ( -32.23382792203229741, 83.71979900898287497, 68.25000000000000000 ) ) ;
#3148 = VECTOR ( 'NONE', #17258, 1000.000000000000000 ) ;
#3149 = AXIS2_PLACEMENT_3D ( 'NONE', #15599, #3654, #7131 ) ;
#3150 = APPLICATION_CONTEXT ( 'automotive_design' ) ;
#3151 = PLANE ( 'NONE',  #8499 ) ;
#3152 = ORIENTED_EDGE ( 'NONE', *, *, #4213, .F. ) ;
#3153 = DIRECTION ( 'NONE',  ( 0.000000000000000000, 0.000000000000000000, -1.000000000000000000 ) ) ;
#3154 = CARTESIAN_POINT ( 'NONE',  ( -1.724728116533986721, 43.31054587065082728, 53.76679706732590347 ) ) ;
#3155 = EDGE_LOOP ( 'NONE', ( #16198, #10574, #3540, #17468 ) ) ;
#3156 = VERTEX_POINT ( 'NONE', #18246 ) ;
#3157 = DIRECTION ( 'NONE',  ( -0.000000000000000000, -0.000000000000000000, -1.000000000000000000 ) ) ;
#3158 = VERTEX_POINT ( 'NONE', #16109 ) ;
#3159 = AXIS2_PLACEMENT_3D ( 'NONE', #9905, #3071, #1268 ) ;
#3160 = CIRCLE ( 'NONE', #12087, 0.5000000000000004441 ) ;
#3161 = DIRECTION ( 'NONE',  ( 1.000000000000000000, 0.000000000000000000, 0.000000000000000000 ) ) ;
#3162 = ORIENTED_EDGE ( 'NONE', *, *, #17189, .T. ) ;
#3163 = ORIENTED_EDGE ( 'NONE', *, *, #14368, .F. ) ;
#3164 = EDGE_CURVE ( 'NONE', #7522, #16140, #18356, .T. ) ;
#3165 = TOROIDAL_SURFACE ( 'NONE', #16377, 5.299999999999999822, 0.2999999999999999889 ) ;
#3166 = ORIENTED_EDGE ( 'NONE', *, *, #2945, .F. ) ;
#3167 = VECTOR ( 'NONE', #6234, 1000.000000000000000 ) ;
#3168 = CARTESIAN_POINT ( 'NONE',  ( 29.37540678000427619, -5.000000000000000000, 3.799999999999999822 ) ) ;
#3169 = DIRECTION ( 'NONE',  ( 0.000000000000000000, 0.000000000000000000, -1.000000000000000000 ) ) ;
#3170 = DIRECTION ( 'NONE',  ( 0.000000000000000000, 0.000000000000000000, 1.000000000000000000 ) ) ;
#3171 = VERTEX_POINT ( 'NONE', #9414 ) ;
#3172 = CARTESIAN_POINT ( 'NONE',  ( -1.824728116533986810, 42.36054587065083155, 53.66679706732590915 ) ) ;
#3173 = EDGE_CURVE ( 'NONE', #16033, #8961, #14072, .T. ) ;
#3174 = DIRECTION ( 'NONE',  ( 0.000000000000000000, 0.000000000000000000, 1.000000000000000000 ) ) ;
#3175 = DIRECTION ( 'NONE',  ( 1.000000000000000000, -0.000000000000000000, 0.000000000000000000 ) ) ;
#3176 = CIRCLE ( 'NONE', #11740, 0.2500000000000002220 ) ;
#3177 = FACE_OUTER_BOUND ( 'NONE', #8828, .T. ) ;
#3178 = PLANE ( 'NONE',  #10786 ) ;
#3179 = VECTOR ( 'NONE', #15581, 1000.000000000000000 ) ;
#3180 = ORIENTED_EDGE ( 'NONE', *, *, #11427, .F. ) ;
#3181 = ORIENTED_EDGE ( 'NONE', *, *, #781, .F. ) ;
#3182 = ORIENTED_EDGE ( 'NONE', *, *, #20735, .T. ) ;
#3183 = CYLINDRICAL_SURFACE ( 'NONE', #13133, 0.2999999999999999334 ) ;
#3184 = TOROIDAL_SURFACE ( 'NONE', #11033, 2.076718556943726313, 0.2500000000000000000 ) ;
#3185 = DIRECTION ( 'NONE',  ( 0.000000000000000000, 0.000000000000000000, 1.000000000000000000 ) ) ;
#3186 = ORIENTED_EDGE ( 'NONE', *, *, #11639, .T. ) ;
#3187 = LINE ( 'NONE', #10671, #21683 ) ;
#3188 = ORIENTED_EDGE ( 'NONE', *, *, #1284, .T. ) ;
#3189 = CARTESIAN_POINT ( 'NONE',  ( -32.20000000000001705, -71.00000000000001421, 1.800000000000000044 ) ) ;
#3190 = DIRECTION ( 'NONE',  ( 1.000000000000000000, 0.000000000000000000, -0.000000000000000000 ) ) ;
#3191 = AXIS2_PLACEMENT_3D ( 'NONE', #1449, #1671, #1 ) ;
#3192 = PLANE ( 'NONE',  #15929 ) ;
#3193 = ORIENTED_EDGE ( 'NONE', *, *, #6213, .T. ) ;
#3194 = DIRECTION ( 'NONE',  ( 0.000000000000000000, 0.000000000000000000, -1.000000000000000000 ) ) ;
#3195 = SPHERICAL_SURFACE ( 'NONE', #1389, 0.2999999999999999889 ) ;
#3196 = ADVANCED_FACE ( 'NONE', ( #1012 ), #21402, .T. ) ;
#3197 = AXIS2_PLACEMENT_3D ( 'NONE', #5832, #19915, #16301 ) ;
#3198 = DIRECTION ( 'NONE',  ( 0.000000000000000000, 0.000000000000000000, 1.000000000000000000 ) ) ;
#3199 = EDGE_CURVE ( 'NONE', #19660, #12157, #2924, .T. ) ;
#3200 = DIRECTION ( 'NONE',  ( 0.000000000000000000, 0.000000000000000000, -1.000000000000000000 ) ) ;
#3201 = LINE ( 'NONE', #20320, #19349 ) ;
#3202 = ORIENTED_EDGE ( 'NONE', *, *, #7717, .T. ) ;
#3203 = CARTESIAN_POINT ( 'NONE',  ( 1.774728116533979660, 42.31054587065082728, 33.66679706732590915 ) ) ;
#3204 = EDGE_LOOP ( 'NONE', ( #15279, #8724, #11068, #17018 ) ) ;
#3205 = CARTESIAN_POINT ( 'NONE',  ( -1.724728116533986721, 43.26054587065083012, 33.76679706732591058 ) ) ;
#3206 = CARTESIAN_POINT ( 'NONE',  ( 30.37540678000427619, 63.74634676501045050, 3.799999999999999822 ) ) ;
#3207 = EDGE_LOOP ( 'NONE', ( #4363, #17940, #19767, #1155, #18757, #12244, #12082, #549, #5858, #8352, #313, #16200, #9657, #16273, #12947, #19912, #16431, #11487, #5818, #4853 ) ) ;
#3208 = ORIENTED_EDGE ( 'NONE', *, *, #7331, .F. ) ;
#3209 = ORIENTED_EDGE ( 'NONE', *, *, #487, .F. ) ;
#3210 = EDGE_CURVE ( 'NONE', #10547, #8171, #20157, .T. ) ;
#3211 = FACE_OUTER_BOUND ( 'NONE', #4765, .T. ) ;
#3212 = AXIS2_PLACEMENT_3D ( 'NONE', #4568, #6045, #9382 ) ;
#3213 = VECTOR ( 'NONE', #16353, 1000.000000000000000 ) ;
#3214 = AXIS2_PLACEMENT_3D ( 'NONE', #7507, #15649, #10947 ) ;
#3215 = ORIENTED_EDGE ( 'NONE', *, *, #6424, .T. ) ;
#3216 = DIRECTION ( 'NONE',  ( 0.000000000000000000, 1.000000000000000000, 0.000000000000000000 ) ) ;
#3217 = VERTEX_POINT ( 'NONE', #4483 ) ;
#3218 = EDGE_CURVE ( 'NONE', #18098, #18442, #3367, .T. ) ;
#3219 = EDGE_LOOP ( 'NONE', ( #15618, #14376, #8373, #15070 ) ) ;
#3220 = CARTESIAN_POINT ( 'NONE',  ( -23.02398829872513986, 7.027230193580998154E-15, 13.79999999999999893 ) ) ;
#3221 = ORIENTED_EDGE ( 'NONE', *, *, #7446, .F. ) ;
#3222 = CARTESIAN_POINT ( 'NONE',  ( -29.20000000000002061, 68.70000000000001705, 0.000000000000000000 ) ) ;
#3223 = LINE ( 'NONE', #12941, #8117 ) ;
#3224 = CARTESIAN_POINT ( 'NONE',  ( 25.37540678000427263, -67.54634676501045476, 7.500000000000000000 ) ) ;
#3225 = CARTESIAN_POINT ( 'NONE',  ( 1.824728116533979705, 43.31054587065082728, 49.66679706732590915 ) ) ;
#3226 = CARTESIAN_POINT ( 'NONE',  ( 26.56227312273159313, -9.958410664601842655, 42.50000000000000000 ) ) ;
#3227 = CIRCLE ( 'NONE', #1074, 0.1000000000000028644 ) ;
#3228 = EDGE_CURVE ( 'NONE', #1963, #341, #18014, .T. ) ;
#3229 = AXIS2_PLACEMENT_3D ( 'NONE', #7143, #19209, #12471 ) ;
#3230 = AXIS2_PLACEMENT_3D ( 'NONE', #19498, #3972, #17817 ) ;
#3231 = EDGE_CURVE ( 'NONE', #17644, #5475, #9521, .T. ) ;
#3232 = CARTESIAN_POINT ( 'NONE',  ( -29.20000000000002061, -2.799282752659324025, 0.000000000000000000 ) ) ;
#3233 = ORIENTED_EDGE ( 'NONE', *, *, #12770, .T. ) ;
#3234 = LINE ( 'NONE', #10163, #7000 ) ;
#3235 = EDGE_CURVE ( 'NONE', #4063, #445, #10511, .T. ) ;
#3236 = CARTESIAN_POINT ( 'NONE',  ( -3.627054932750481964, -32.61873716947361856, 68.00000000000000000 ) ) ;
#3237 = ORIENTED_EDGE ( 'NONE', *, *, #16885, .T. ) ;
#3238 = CARTESIAN_POINT ( 'NONE',  ( -25.37540678000427263, 69.04634676501045476, 3.799999999999999822 ) ) ;
#3239 = LINE ( 'NONE', #10067, #10308 ) ;
#3240 = VERTEX_POINT ( 'NONE', #11296 ) ;
#3241 = ORIENTED_EDGE ( 'NONE', *, *, #9266, .T. ) ;
#3242 = DIRECTION ( 'NONE',  ( 0.000000000000000000, 0.000000000000000000, -1.000000000000000000 ) ) ;
#3243 = AXIS2_PLACEMENT_3D ( 'NONE', #11895, #8335, #15142 ) ;
#3244 = EDGE_CURVE ( 'NONE', #17577, #12310, #4435, .T. ) ;
#3245 = CIRCLE ( 'NONE', #13245, 0.1000000000000028644 ) ;
#3246 = ORIENTED_EDGE ( 'NONE', *, *, #19839, .T. ) ;
#3247 = DIRECTION ( 'NONE',  ( -1.000000000000000000, -0.000000000000000000, -0.000000000000000000 ) ) ;
#3248 = ORIENTED_EDGE ( 'NONE', *, *, #20859, .T. ) ;
#3249 = CARTESIAN_POINT ( 'NONE',  ( -31.50000000000002132, -71.00000000000001421, 1.800000000000000044 ) ) ;
#3250 = DIRECTION ( 'NONE',  ( 1.000000000000000000, 0.000000000000000000, 0.000000000000000000 ) ) ;
#3251 = EDGE_CURVE ( 'NONE', #497, #18691, #489, .T. ) ;
#3252 = FACE_OUTER_BOUND ( 'NONE', #7984, .T. ) ;
#3253 = LINE ( 'NONE', #11957, #3979 ) ;
#3254 = EDGE_CURVE ( 'NONE', #16058, #12787, #11932, .T. ) ;
#3255 = CIRCLE ( 'NONE', #19342, 4.051418481279135619 ) ;
#3256 = CARTESIAN_POINT ( 'NONE',  ( -30.07540678000427548, 6.000000000000000000, 7.200000000000000178 ) ) ;
#3257 = FACE_OUTER_BOUND ( 'NONE', #191, .T. ) ;
#3258 = DIRECTION ( 'NONE',  ( 1.224646799147353207E-16, 0.000000000000000000, 1.000000000000000000 ) ) ;
#3259 = FACE_OUTER_BOUND ( 'NONE', #720, .T. ) ;
#3260 = VERTEX_POINT ( 'NONE', #1673 ) ;
#3261 = DIRECTION ( 'NONE',  ( 0.000000000000000000, -1.000000000000000000, 0.000000000000000000 ) ) ;
#3262 = VERTEX_POINT ( 'NONE', #6520 ) ;
#3263 = VERTEX_POINT ( 'NONE', #112 ) ;
#3264 = LINE ( 'NONE', #17012, #3537 ) ;
#3265 = DIRECTION ( 'NONE',  ( 1.000000000000000000, 0.000000000000000000, 0.000000000000000000 ) ) ;
#3266 = AXIS2_PLACEMENT_3D ( 'NONE', #4769, #19999, #11572 ) ;
#3267 = ORIENTED_EDGE ( 'NONE', *, *, #10098, .T. ) ;
#3268 = CIRCLE ( 'NONE', #2917, 1.999999999999991340 ) ;
#3269 =( BOUNDED_CURVE ( )  B_SPLINE_CURVE ( 3, ( #13677, #18955, #18611, #3625 ),
 .UNSPECIFIED., .F., .T. ) 
 B_SPLINE_CURVE_WITH_KNOTS ( ( 4, 4 ),
 ( 3.141592653589746931, 4.712388980384689674 ),
 .UNSPECIFIED. ) 
 CURVE ( )  GEOMETRIC_REPRESENTATION_ITEM ( )  RATIONAL_B_SPLINE_CURVE ( ( 1.000000000000000000, 0.8047378541243541683, 0.8047378541243541683, 1.000000000000000000 ) ) 
 REPRESENTATION_ITEM ( '' )  );
#3270 = SURFACE_STYLE_USAGE ( .BOTH. , #19725 ) ;
#3271 = EDGE_CURVE ( 'NONE', #573, #7129, #6599, .T. ) ;
#3272 = ORIENTED_EDGE ( 'NONE', *, *, #19757, .T. ) ;
#3273 = AXIS2_PLACEMENT_3D ( 'NONE', #10904, #5685, #7464 ) ;
#3274 = EDGE_CURVE ( 'NONE', #7310, #12787, #15140, .T. ) ;
#3275 = EDGE_LOOP ( 'NONE', ( #11869, #3310, #5036, #12665 ) ) ;
#3276 = DIRECTION ( 'NONE',  ( 0.000000000000000000, 0.000000000000000000, -1.000000000000000000 ) ) ;
#3277 = CYLINDRICAL_SURFACE ( 'NONE', #2038, 0.6000000000000033085 ) ;
#3278 = CIRCLE ( 'NONE', #7565, 0.1000000000000028644 ) ;
#3279 = CARTESIAN_POINT ( 'NONE',  ( 34.39999999999998437, -85.00000000000000000, 0.6000000000000041966 ) ) ;
#3280 = CARTESIAN_POINT ( 'NONE',  ( 31.69597781366222122, 27.99124249474150972, 70.50000000000000000 ) ) ;
#3281 = ORIENTED_EDGE ( 'NONE', *, *, #21219, .F. ) ;
#3282 = DIRECTION ( 'NONE',  ( 0.000000000000000000, 0.000000000000000000, -1.000000000000000000 ) ) ;
#3283 = ADVANCED_FACE ( 'NONE', ( #11959 ), #9857, .F. ) ;
#3284 = DIRECTION ( 'NONE',  ( -1.000000000000000000, 0.000000000000000000, 0.000000000000000000 ) ) ;
#3285 = CIRCLE ( 'NONE', #13289, 0.2999999999999999889 ) ;
#3286 = FACE_OUTER_BOUND ( 'NONE', #17670, .T. ) ;
#3287 = FACE_OUTER_BOUND ( 'NONE', #21478, .T. ) ;
#3288 = CARTESIAN_POINT ( 'NONE',  ( -8.134906293162361024, 41.92645089659918511, 68.06527860057354928 ) ) ;
#3289 = VERTEX_POINT ( 'NONE', #10186 ) ;
#3290 = EDGE_LOOP ( 'NONE', ( #14582, #17613, #13227, #20690 ) ) ;
#3291 = EDGE_LOOP ( 'NONE', ( #10644, #3095, #16394, #3422 ) ) ;
#3292 = DIRECTION ( 'NONE',  ( -0.000000000000000000, -0.000000000000000000, -1.000000000000000000 ) ) ;
#3293 = CARTESIAN_POINT ( 'NONE',  ( -29.20000000000002061, -2.799282752659324025, 0.000000000000000000 ) ) ;
#3294 = EDGE_LOOP ( 'NONE', ( #3624, #10727, #3964, #13933, #16073 ) ) ;
#3295 = FACE_OUTER_BOUND ( 'NONE', #17576, .T. ) ;
#3296 = CIRCLE ( 'NONE', #19379, 1.000000000000000888 ) ;
#3297 = CIRCLE ( 'NONE', #19022, 0.5000000000000004441 ) ;
#3298 = ORIENTED_EDGE ( 'NONE', *, *, #16069, .T. ) ;
#3299 = CARTESIAN_POINT ( 'NONE',  ( 1.724728116533979838, 43.31054587065082728, 49.66679706732590915 ) ) ;
#3300 = EDGE_CURVE ( 'NONE', #19588, #13533, #2288, .T. ) ;
#3301 = DIRECTION ( 'NONE',  ( -0.000000000000000000, -0.000000000000000000, -1.000000000000000000 ) ) ;
#3302 = DIRECTION ( 'NONE',  ( 0.000000000000000000, 0.000000000000000000, 1.000000000000000000 ) ) ;
#3303 = CARTESIAN_POINT ( 'NONE',  ( 0.000000000000000000, -69.00000000000000000, 0.2999999999999947153 ) ) ;
#3304 = ORIENTED_EDGE ( 'NONE', *, *, #2620, .F. ) ;
#3305 = DIRECTION ( 'NONE',  ( -0.000000000000000000, 0.000000000000000000, 1.000000000000000000 ) ) ;
#3306 = FACE_OUTER_BOUND ( 'NONE', #18783, .T. ) ;
#3307 = CARTESIAN_POINT ( 'NONE',  ( -15.95292532278785913, 32.11873716947361856, 42.50000000000000711 ) ) ;
#3308 = DIRECTION ( 'NONE',  ( -1.000000000000000000, 0.000000000000000000, 0.000000000000000000 ) ) ;
#3309 = LINE ( 'NONE', #10468, #20425 ) ;
#3310 = ORIENTED_EDGE ( 'NONE', *, *, #7013, .F. ) ;
#3311 = CARTESIAN_POINT ( 'NONE',  ( -15.95292532278785913, -52.39333383871510108, 13.79999999999999716 ) ) ;
#3312 = VECTOR ( 'NONE', #13862, 1000.000000000000000 ) ;
#3313 = ORIENTED_EDGE ( 'NONE', *, *, #12905, .T. ) ;
#3314 = CARTESIAN_POINT ( 'NONE',  ( 13.37248138918699425, 42.46645089659917716, 68.50000000000000000 ) ) ;
#3315 = AXIS2_PLACEMENT_3D ( 'NONE', #21460, #9802, #20105 ) ;
#3316 = CARTESIAN_POINT ( 'NONE',  ( -14.96174975910705207, -42.31054587065082728, 68.25000000000000000 ) ) ;
#3317 = EDGE_CURVE ( 'NONE', #7284, #14159, #18000, .T. ) ;
#3318 = ORIENTED_EDGE ( 'NONE', *, *, #14610, .F. ) ;
#3319 = EDGE_LOOP ( 'NONE', ( #11753, #21197, #21247, #19836 ) ) ;
#3320 = ORIENTED_EDGE ( 'NONE', *, *, #8209, .F. ) ;
#3321 = DIRECTION ( 'NONE',  ( 0.000000000000000000, 0.000000000000000000, 1.000000000000000000 ) ) ;
#3322 = FACE_OUTER_BOUND ( 'NONE', #20839, .T. ) ;
#3323 = ORIENTED_EDGE ( 'NONE', *, *, #4879, .T. ) ;
#3324 = AXIS2_PLACEMENT_3D ( 'NONE', #6880, #13335, #15027 ) ;
#3325 = EDGE_CURVE ( 'NONE', #9625, #1254, #20494, .T. ) ;
#3326 = ORIENTED_EDGE ( 'NONE', *, *, #15555, .F. ) ;
#3327 = VERTEX_POINT ( 'NONE', #20151 ) ;
#3328 = DIRECTION ( 'NONE',  ( -1.000000000000000000, -0.000000000000000000, 0.000000000000000000 ) ) ;
#3329 = VERTEX_POINT ( 'NONE', #13543 ) ;
#3330 = CARTESIAN_POINT ( 'NONE',  ( 1.724728116533978728, 43.31054587065082728, 41.71679706732590631 ) ) ;
#3331 = FACE_OUTER_BOUND ( 'NONE', #7926, .T. ) ;
#3332 = DIRECTION ( 'NONE',  ( -1.000000000000000000, 0.000000000000000000, 1.224646799147353207E-16 ) ) ;
#3333 = CYLINDRICAL_SURFACE ( 'NONE', #15912, 0.3000000000000016542 ) ;
#3334 = ORIENTED_EDGE ( 'NONE', *, *, #10865, .F. ) ;
#3335 = CARTESIAN_POINT ( 'NONE',  ( 28.87540678000427619, -6.494748934539263274, 7.799999999999999822 ) ) ;
#3336 = LINE ( 'NONE', #8368, #16010 ) ;
#3337 = DIRECTION ( 'NONE',  ( 0.9729678061520345977, 0.2309407893631976461, 0.000000000000000000 ) ) ;
#3338 = CARTESIAN_POINT ( 'NONE',  ( 23.32398829872514057, 5.683640910026983128, 13.50000000000000000 ) ) ;
#3339 = ORIENTED_EDGE ( 'NONE', *, *, #1200, .T. ) ;
#3340 = DIRECTION ( 'NONE',  ( -2.388292521039847891E-16, 0.000000000000000000, -1.000000000000000000 ) ) ;
#3341 = EDGE_CURVE ( 'NONE', #8501, #18098, #9084, .T. ) ;
#3342 = ORIENTED_EDGE ( 'NONE', *, *, #11310, .F. ) ;
#3343 = DIRECTION ( 'NONE',  ( -0.000000000000000000, 1.000000000000000000, -0.000000000000000000 ) ) ;
#3344 = FACE_OUTER_BOUND ( 'NONE', #19612, .T. ) ;
#3345 = ORIENTED_EDGE ( 'NONE', *, *, #11344, .T. ) ;
#3346 = ORIENTED_EDGE ( 'NONE', *, *, #2648, .T. ) ;
#3347 = EDGE_CURVE ( 'NONE', #2915, #675, #7303, .T. ) ;
#3348 = EDGE_CURVE ( 'NONE', #124, #17663, #1794, .T. ) ;
#3349 = ORIENTED_EDGE ( 'NONE', *, *, #143, .T. ) ;
#3350 = DIRECTION ( 'NONE',  ( -1.000000000000000000, 0.000000000000000000, 0.000000000000000000 ) ) ;
#3351 = ORIENTED_EDGE ( 'NONE', *, *, #11911, .F. ) ;
#3352 = LINE ( 'NONE', #6952, #7777 ) ;
#3353 = DIRECTION ( 'NONE',  ( -1.224646799147353207E-16, 0.000000000000000000, -1.000000000000000000 ) ) ;
#3354 = CARTESIAN_POINT ( 'NONE',  ( -8.638906393579159015, 43.49585613540820361, 70.88527860057354246 ) ) ;
#3355 = FACE_OUTER_BOUND ( 'NONE', #4465, .T. ) ;
#3356 = DIRECTION ( 'NONE',  ( 1.000000000000000000, 0.000000000000000000, 0.000000000000000000 ) ) ;
#3357 = DIRECTION ( 'NONE',  ( -0.000000000000000000, -0.000000000000000000, 1.000000000000000000 ) ) ;
#3358 = ADVANCED_FACE ( 'NONE', ( #20382 ), #8631, .T. ) ;
#3359 = CIRCLE ( 'NONE', #15848, 0.2999999999999999334 ) ;
#3360 = DIRECTION ( 'NONE',  ( 0.000000000000000000, 0.000000000000000000, 1.000000000000000000 ) ) ;
#3361 = CARTESIAN_POINT ( 'NONE',  ( 1.824728116533979261, 43.31054587065082728, 31.70876104995653932 ) ) ;
#3362 = FACE_OUTER_BOUND ( 'NONE', #9982, .T. ) ;
#3363 = ORIENTED_EDGE ( 'NONE', *, *, #19287, .T. ) ;
#3364 = DIRECTION ( 'NONE',  ( 0.9729678061520319332, 0.2309407893632090258, 0.000000000000000000 ) ) ;
#3365 = ORIENTED_EDGE ( 'NONE', *, *, #18336, .F. ) ;
#3366 = LINE ( 'NONE', #13213, #14867 ) ;
#3367 = CIRCLE ( 'NONE', #1916, 4.351418481279137218 ) ;
#3368 = EDGE_LOOP ( 'NONE', ( #14010, #13030, #5863, #4979, #15932, #21744, #4489, #17017 ) ) ;
#3369 = VECTOR ( 'NONE', #14023, 1000.000000000000000 ) ;
#3370 = ORIENTED_EDGE ( 'NONE', *, *, #18965, .T. ) ;
#3371 = DIRECTION ( 'NONE',  ( -0.000000000000000000, -0.000000000000000000, -1.000000000000000000 ) ) ;
#3372 = DIRECTION ( 'NONE',  ( 0.000000000000000000, 0.000000000000000000, -1.000000000000000000 ) ) ;
#3373 = ADVANCED_FACE ( 'NONE', ( #11524 ), #21845, .T. ) ;
#3374 = ORIENTED_EDGE ( 'NONE', *, *, #10981, .F. ) ;
#3375 = EDGE_CURVE ( 'NONE', #11863, #7877, #2642, .T. ) ;
#3376 = ADVANCED_FACE ( 'NONE', ( #1452 ), #5520, .T. ) ;
#3377 = EDGE_LOOP ( 'NONE', ( #21208, #3401, #18696, #15393 ) ) ;
#3378 = ORIENTED_EDGE ( 'NONE', *, *, #10066, .F. ) ;
#3379 = DIRECTION ( 'NONE',  ( 0.000000000000000000, 1.000000000000000000, -0.000000000000000000 ) ) ;
#3380 = CARTESIAN_POINT ( 'NONE',  ( -11.62890639357915923, 43.00645089659917630, 70.88527860057354246 ) ) ;
#3381 = CYLINDRICAL_SURFACE ( 'NONE', #10424, 0.5000000000000004441 ) ;
#3382 = DIRECTION ( 'NONE',  ( 0.000000000000000000, 0.000000000000000000, -1.000000000000000000 ) ) ;
#3383 = AXIS2_PLACEMENT_3D ( 'NONE', #15467, #6885, #10542 ) ;
#3384 = DIRECTION ( 'NONE',  ( 0.000000000000000000, 1.000000000000000000, -0.000000000000000000 ) ) ;
#3385 = DIRECTION ( 'NONE',  ( -0.000000000000000000, 1.000000000000000000, -0.000000000000000000 ) ) ;
#3386 = CARTESIAN_POINT ( 'NONE',  ( 27.67540678000428045, 7.839012376739720627E-15, 13.79999999999999893 ) ) ;
#3387 = DIRECTION ( 'NONE',  ( -1.000000000000000000, 0.000000000000000000, 0.000000000000000000 ) ) ;
#3388 = CARTESIAN_POINT ( 'NONE',  ( -1.774728116533986544, 43.31054587065082728, 43.80876104995653719 ) ) ;
#3389 = EDGE_CURVE ( 'NONE', #1657, #8381, #21948, .T. ) ;
#3390 = CARTESIAN_POINT ( 'NONE',  ( -1.824728116533986810, 42.36054587065083155, 49.76679706732591058 ) ) ;
#3391 = EDGE_LOOP ( 'NONE', ( #8764, #10759, #6632, #13826 ) ) ;
#3392 = ORIENTED_EDGE ( 'NONE', *, *, #4858, .F. ) ;
#3393 = ORIENTED_EDGE ( 'NONE', *, *, #12383, .F. ) ;
#3394 = CARTESIAN_POINT ( 'NONE',  ( -33.80000000000000426, 85.00000000000000000, 1.500000000000001332 ) ) ;
#3395 =( NAMED_UNIT ( * ) PLANE_ANGLE_UNIT ( ) SI_UNIT ( $, .RADIAN. ) );
#3396 = CARTESIAN_POINT ( 'NONE',  ( -1.824728116533986810, 43.26054587065083012, 51.80876104995653719 ) ) ;
#3397 = ORIENTED_EDGE ( 'NONE', *, *, #7908, .T. ) ;
#3398 = CIRCLE ( 'NONE', #21279, 0.2999999999999999334 ) ;
#3399 = DIRECTION ( 'NONE',  ( 0.000000000000000000, 0.000000000000000000, 1.000000000000000000 ) ) ;
#3400 = PRESENTATION_LAYER_ASSIGNMENT (  '', '', ( #522 ) ) ;
#3401 = ORIENTED_EDGE ( 'NONE', *, *, #8232, .F. ) ;
#3402 = ADVANCED_FACE ( 'NONE', ( #8954 ), #3928, .T. ) ;
#3403 = EDGE_LOOP ( 'NONE', ( #10006, #6323, #7621, #7260 ) ) ;
#3404 = DIRECTION ( 'NONE',  ( 1.000000000000000000, 0.000000000000000000, 0.000000000000000000 ) ) ;
#3405 = CARTESIAN_POINT ( 'NONE',  ( -23.61959064016851073, 45.26242829375641463, 68.50000000000000000 ) ) ;
#3406 = DIRECTION ( 'NONE',  ( 0.000000000000000000, 0.000000000000000000, 1.000000000000000000 ) ) ;
#3407 = CIRCLE ( 'NONE', #15890, 2.767785046117004377 ) ;
#3408 = ORIENTED_EDGE ( 'NONE', *, *, #6784, .T. ) ;
#3409 = CARTESIAN_POINT ( 'NONE',  ( 18.22752199202934520, 38.74634676501045760, 13.50000000000000000 ) ) ;
#3410 = DIRECTION ( 'NONE',  ( 0.000000000000000000, 0.000000000000000000, 1.000000000000000000 ) ) ;
#3411 = CARTESIAN_POINT ( 'NONE',  ( -33.50000000000001421, -85.00000000000000000, 78.20000000000000284 ) ) ;
#3412 = FACE_OUTER_BOUND ( 'NONE', #19014, .T. ) ;
#3413 = ORIENTED_EDGE ( 'NONE', *, *, #3492, .T. ) ;
#3414 = DIRECTION ( 'NONE',  ( 0.000000000000000000, 0.000000000000000000, 1.000000000000000000 ) ) ;
#3415 = AXIS2_PLACEMENT_3D ( 'NONE', #2981, #14385, #16271 ) ;
#3416 = VECTOR ( 'NONE', #9438, 1000.000000000000000 ) ;
#3417 = ADVANCED_FACE ( 'NONE', ( #15532, #21046 ), #2227, .F. ) ;
#3418 = EDGE_LOOP ( 'NONE', ( #16905, #13400, #6180, #10258 ) ) ;
#3419 = CARTESIAN_POINT ( 'NONE',  ( -1.824728116533986810, 42.36054587065083155, 47.70876104995654288 ) ) ;
#3420 = DIRECTION ( 'NONE',  ( -1.000000000000000000, -5.192538640813645496E-17, 7.145994714117440585E-17 ) ) ;
#3421 = CARTESIAN_POINT ( 'NONE',  ( 1.824728116533979261, 42.36054587065083155, 47.80876104995653719 ) ) ;
#3422 = ORIENTED_EDGE ( 'NONE', *, *, #15194, .F. ) ;
#3423 = EDGE_LOOP ( 'NONE', ( #11175, #4783, #12878, #18896 ) ) ;
#3424 = EDGE_LOOP ( 'NONE', ( #10140, #16440, #9658, #1663 ) ) ;
#3425 = CARTESIAN_POINT ( 'NONE',  ( -14.96174975910705207, 51.61873716947361856, 14.00000000000000000 ) ) ;
#3426 = CYLINDRICAL_SURFACE ( 'NONE', #21092, 0.3000000000000016542 ) ;
#3427 = EDGE_LOOP ( 'NONE', ( #19693, #15433, #2178, #18069 ) ) ;
#3428 = PLANE ( 'NONE',  #3498 ) ;
#3429 = VECTOR ( 'NONE', #19814, 1000.000000000000000 ) ;
#3430 = ORIENTED_EDGE ( 'NONE', *, *, #19615, .F. ) ;
#3431 = CARTESIAN_POINT ( 'NONE',  ( -34.40000000000001279, -85.00000000000000000, 79.70000000000000284 ) ) ;
#3432 = AXIS2_PLACEMENT_3D ( 'NONE', #15993, #3825, #19469 ) ;
#3433 = TOROIDAL_SURFACE ( 'NONE', #15524, 1.300000000000000044, 0.2999999999999999889 ) ;
#3434 = CIRCLE ( 'NONE', #9131, 0.2999999999999999334 ) ;
#3435 = EDGE_LOOP ( 'NONE', ( #5947, #12267, #16933, #6581 ) ) ;
#3436 = DIRECTION ( 'NONE',  ( -1.000000000000000000, 0.000000000000000000, 0.000000000000000000 ) ) ;
#3437 = DIRECTION ( 'NONE',  ( 1.000000000000000000, 0.000000000000000000, 0.000000000000000000 ) ) ;
#3438 = ADVANCED_FACE ( 'NONE', ( #10744 ), #1894, .T. ) ;
#3439 = CARTESIAN_POINT ( 'NONE',  ( -34.39999999999999858, -84.70000000000001705, 0.3000000000000033196 ) ) ;
#3440 = DIRECTION ( 'NONE',  ( -0.000000000000000000, -1.000000000000000000, -0.000000000000000000 ) ) ;
#3441 = ORIENTED_EDGE ( 'NONE', *, *, #19638, .T. ) ;
#3442 = CARTESIAN_POINT ( 'NONE',  ( 23.10708008847558759, 2.595912616485783087, 13.38952209624200584 ) ) ;
#3443 = LINE ( 'NONE', #1641, #9245 ) ;
#3444 = CARTESIAN_POINT ( 'NONE',  ( -25.37540678000427263, 68.74634676501045760, 7.200000000000000178 ) ) ;
#3445 = ORIENTED_EDGE ( 'NONE', *, *, #18026, .T. ) ;
#3446 = AXIS2_PLACEMENT_3D ( 'NONE', #21278, #18124, #12740 ) ;
#3447 = CIRCLE ( 'NONE', #9159, 0.2500000000000002220 ) ;
#3448 = CARTESIAN_POINT ( 'NONE',  ( 30.19999999999999574, 70.00000000000000000, 1.500000000000004885 ) ) ;
#3449 = AXIS2_PLACEMENT_3D ( 'NONE', #19594, #12527, #14325 ) ;
#3450 = ADVANCED_FACE ( 'NONE', ( #20711 ), #325, .T. ) ;
#3451 = DIRECTION ( 'NONE',  ( 1.000000000000000000, 0.000000000000000000, 0.000000000000000000 ) ) ;
#3452 = ORIENTED_EDGE ( 'NONE', *, *, #4311, .F. ) ;
#3453 = CIRCLE ( 'NONE', #18081, 0.5000000000000004441 ) ;
#3454 = DIRECTION ( 'NONE',  ( 0.000000000000000000, -0.000000000000000000, 1.000000000000000000 ) ) ;
#3455 = FACE_OUTER_BOUND ( 'NONE', #20544, .T. ) ;
#3456 = ORIENTED_EDGE ( 'NONE', *, *, #5639, .T. ) ;
#3457 = ORIENTED_EDGE ( 'NONE', *, *, #13316, .F. ) ;
#3458 = DIRECTION ( 'NONE',  ( 1.000000000000000000, 0.000000000000000000, 0.000000000000000000 ) ) ;
#3459 = ORIENTED_EDGE ( 'NONE', *, *, #21583, .F. ) ;
#3460 = AXIS2_PLACEMENT_3D ( 'NONE', #14713, #4657, #17959 ) ;
#3461 = VECTOR ( 'NONE', #3084, 1000.000000000000000 ) ;
#3462 = AXIS2_PLACEMENT_3D ( 'NONE', #2586, #1003, #6072 ) ;
#3463 = EDGE_CURVE ( 'NONE', #14452, #6925, #10416, .T. ) ;
#3464 = DIRECTION ( 'NONE',  ( -0.000000000000000000, 1.000000000000000000, 0.000000000000000000 ) ) ;
#3465 = ORIENTED_EDGE ( 'NONE', *, *, #8473, .T. ) ;
#3466 = CARTESIAN_POINT ( 'NONE',  ( 23.02398829872513986, 7.027230193580998154E-15, 13.79999999999999893 ) ) ;
#3467 = CIRCLE ( 'NONE', #9532, 0.5000000000000004441 ) ;
#3468 = FACE_OUTER_BOUND ( 'NONE', #21574, .T. ) ;
#3469 = DIRECTION ( 'NONE',  ( 0.000000000000000000, 0.000000000000000000, 1.000000000000000000 ) ) ;
#3470 = CARTESIAN_POINT ( 'NONE',  ( -1.824728116533986810, 42.36054587065083155, 37.66679706732590915 ) ) ;
#3471 = EDGE_CURVE ( 'NONE', #11153, #2242, #17823, .T. ) ;
#3472 = EDGE_CURVE ( 'NONE', #16612, #16887, #12452, .T. ) ;
#3473 = CARTESIAN_POINT ( 'NONE',  ( -30.79999999999999005, 69.70000000000001705, 0.2999999999999999334 ) ) ;
#3474 = AXIS2_PLACEMENT_3D ( 'NONE', #11874, #1475, #4738 ) ;
#3475 = ADVANCED_FACE ( 'NONE', ( #7175 ), #12176, .F. ) ;
#3476 = CARTESIAN_POINT ( 'NONE',  ( -15.04741597961255728, -51.92573430214628871, 13.50000000000006750 ) ) ;
#3477 = CIRCLE ( 'NONE', #15958, 2.000000000000000000 ) ;
#3478 = VECTOR ( 'NONE', #11113, 1000.000000000000000 ) ;
#3479 = AXIS2_PLACEMENT_3D ( 'NONE', #5245, #15307, #5025 ) ;
#3480 = CARTESIAN_POINT ( 'NONE',  ( -29.17540678000427690, 63.74634676501045050, 7.500000000000000000 ) ) ;
#3481 = LINE ( 'NONE', #11754, #20253 ) ;
#3482 = AXIS2_PLACEMENT_3D ( 'NONE', #8882, #19062, #17484 ) ;
#3483 = DIRECTION ( 'NONE',  ( -0.000000000000000000, -0.000000000000000000, -1.000000000000000000 ) ) ;
#3484 = ORIENTED_EDGE ( 'NONE', *, *, #18523, .T. ) ;
#3485 = AXIS2_PLACEMENT_3D ( 'NONE', #7130, #20212, #4887 ) ;
#3486 = VERTEX_POINT ( 'NONE', #13969 ) ;
#3487 = FACE_OUTER_BOUND ( 'NONE', #12812, .T. ) ;
#3488 = DIRECTION ( 'NONE',  ( 0.000000000000000000, 0.000000000000000000, -1.000000000000000000 ) ) ;
#3489 = VERTEX_POINT ( 'NONE', #8736 ) ;
#3490 = SURFACE_SIDE_STYLE ('',( #15116 ) ) ;
#3491 = ORIENTED_EDGE ( 'NONE', *, *, #13198, .F. ) ;
#3492 = EDGE_CURVE ( 'NONE', #8743, #13557, #5354, .T. ) ;
#3493 = ORIENTED_EDGE ( 'NONE', *, *, #17810, .F. ) ;
#3494 = AXIS2_PLACEMENT_3D ( 'NONE', #15072, #2772, #12938 ) ;
#3495 = CIRCLE ( 'NONE', #3126, 0.2999999999999999334 ) ;
#3496 = CARTESIAN_POINT ( 'NONE',  ( -4.127054932750482408, -32.93424481021354921, 7.321391277662001151 ) ) ;
#3497 = CARTESIAN_POINT ( 'NONE',  ( 9.641460742840918030, -32.61873716947361856, 68.00000000000000000 ) ) ;
#3498 = AXIS2_PLACEMENT_3D ( 'NONE', #5120, #1627, #15286 ) ;
#3499 = DIRECTION ( 'NONE',  ( 0.000000000000000000, -0.000000000000000000, -1.000000000000000000 ) ) ;
#3500 = AXIS2_PLACEMENT_3D ( 'NONE', #16487, #1153, #6445 ) ;
#3501 = DIRECTION ( 'NONE',  ( 0.000000000000000000, -0.000000000000000000, 1.000000000000000000 ) ) ;
#3502 = CIRCLE ( 'NONE', #12767, 0.09999999999999939493 ) ;
#3503 = EDGE_CURVE ( 'NONE', #7899, #471, #2834, .T. ) ;
#3504 = CARTESIAN_POINT ( 'NONE',  ( 15.95292532278785913, 50.11873716947361856, 13.79999999999999893 ) ) ;
#3505 = EDGE_CURVE ( 'NONE', #9791, #6172, #18923, .T. ) ;
#3506 = CARTESIAN_POINT ( 'NONE',  ( -23.36078716634399655, 44.83461903493144973, 13.50000000000000000 ) ) ;
#3507 = CARTESIAN_POINT ( 'NONE',  ( 23.21392692125925450, -3.086569931169083514, 13.48002932626963712 ) ) ;
#3508 = CYLINDRICAL_SURFACE ( 'NONE', #9653, 0.2999999999999999334 ) ;
#3509 = EDGE_CURVE ( 'NONE', #104, #20269, #5716, .T. ) ;
#3510 = DIRECTION ( 'NONE',  ( 0.000000000000000000, 0.000000000000000000, 1.000000000000000000 ) ) ;
#3511 = AXIS2_PLACEMENT_3D ( 'NONE', #20677, #5356, #2079 ) ;
#3512 = AXIS2_PLACEMENT_3D ( 'NONE', #18669, #16766, #18560 ) ;
#3513 = ORIENTED_EDGE ( 'NONE', *, *, #4482, .T. ) ;
#3514 = VERTEX_POINT ( 'NONE', #19029 ) ;
#3515 = DIRECTION ( 'NONE',  ( -1.000000000000000000, 0.000000000000000000, 0.000000000000000000 ) ) ;
#3516 = PRESENTATION_STYLE_ASSIGNMENT (( #17483 ) ) ;
#3517 = DIRECTION ( 'NONE',  ( 0.000000000000000000, 0.000000000000000000, 1.000000000000000000 ) ) ;
#3518 = ORIENTED_EDGE ( 'NONE', *, *, #5988, .F. ) ;
#3519 = DIRECTION ( 'NONE',  ( 0.000000000000000000, 0.000000000000000000, 1.000000000000000000 ) ) ;
#3520 = AXIS2_PLACEMENT_3D ( 'NONE', #15342, #15219, #18473 ) ;
#3521 = CIRCLE ( 'NONE', #17434, 0.3000000000000003775 ) ;
#3522 = ADVANCED_FACE ( 'NONE', ( #4032 ), #4625, .T. ) ;
#3523 = CARTESIAN_POINT ( 'NONE',  ( -14.66174975910705136, -42.11054587065083155, 13.50000000000000000 ) ) ;
#3524 = EDGE_CURVE ( 'NONE', #8381, #225, #9626, .T. ) ;
#3525 = DIRECTION ( 'NONE',  ( 1.000000000000000000, 0.000000000000000000, 0.000000000000000000 ) ) ;
#3526 = CIRCLE ( 'NONE', #6034, 4.700000000000002842 ) ;
#3527 = CARTESIAN_POINT ( 'NONE',  ( 15.95292532278785913, -50.11873716947361856, 13.99999999999999822 ) ) ;
#3528 = ORIENTED_EDGE ( 'NONE', *, *, #17174, .F. ) ;
#3529 = DIRECTION ( 'NONE',  ( -0.000000000000000000, -0.000000000000000000, -1.000000000000000000 ) ) ;
#3530 = PLANE ( 'NONE',  #13539 ) ;
#3531 = CARTESIAN_POINT ( 'NONE',  ( -3.627054932750481964, 32.93424481021354921, 42.50000000000000000 ) ) ;
#3532 = VECTOR ( 'NONE', #21595, 1000.000000000000000 ) ;
#3533 = DIRECTION ( 'NONE',  ( 0.000000000000000000, 1.000000000000000000, 0.000000000000000000 ) ) ;
#3534 = CARTESIAN_POINT ( 'NONE',  ( -1.724728116533986721, 42.36054587065083155, 35.80876104995653009 ) ) ;
#3535 = CARTESIAN_POINT ( 'NONE',  ( 15.95292532278785913, -32.61873716947361856, 68.50000000000000000 ) ) ;
#3536 = CIRCLE ( 'NONE', #3482, 3.017785046117004377 ) ;
#3537 = VECTOR ( 'NONE', #20272, 1000.000000000000000 ) ;
#3538 = VECTOR ( 'NONE', #19113, 1000.000000000000000 ) ;
#3539 = ADVANCED_FACE ( 'NONE', ( #15971 ), #11401, .T. ) ;
#3540 = ORIENTED_EDGE ( 'NONE', *, *, #19585, .F. ) ;
#3541 = DIRECTION ( 'NONE',  ( 0.000000000000000000, 0.000000000000000000, 1.000000000000000000 ) ) ;
#3542 = CARTESIAN_POINT ( 'NONE',  ( -1.774728116533986544, 43.26054587065083012, 43.80876104995653719 ) ) ;
#3543 = FACE_OUTER_BOUND ( 'NONE', #8564, .T. ) ;
#3544 = ORIENTED_EDGE ( 'NONE', *, *, #6618, .T. ) ;
#3545 = ORIENTED_EDGE ( 'NONE', *, *, #35, .F. ) ;
#3546 = ORIENTED_EDGE ( 'NONE', *, *, #11006, .F. ) ;
#3547 = DIRECTION ( 'NONE',  ( -0.000000000000000000, -1.000000000000000000, -0.000000000000000000 ) ) ;
#3548 = CARTESIAN_POINT ( 'NONE',  ( -1.724728116533986721, 43.26054587065083012, 49.76679706732591058 ) ) ;
#3549 = FACE_OUTER_BOUND ( 'NONE', #950, .T. ) ;
#3550 = AXIS2_PLACEMENT_3D ( 'NONE', #17534, #2423, #19428 ) ;
#3551 = DIRECTION ( 'NONE',  ( 0.000000000000000000, 0.000000000000000000, -1.000000000000000000 ) ) ;
#3552 = CIRCLE ( 'NONE', #12108, 0.5000000000000004441 ) ;
#3553 = EDGE_LOOP ( 'NONE', ( #8858, #13895, #9021, #19310 ) ) ;
#3554 = LINE ( 'NONE', #168, #16832 ) ;
#3555 = CIRCLE ( 'NONE', #21787, 0.04999999999999991257 ) ;
#3556 = EDGE_CURVE ( 'NONE', #5726, #5063, #17325, .T. ) ;
#3557 = ORIENTED_EDGE ( 'NONE', *, *, #5875, .T. ) ;
#3558 = CARTESIAN_POINT ( 'NONE',  ( -23.02398829872513986, -3.005406968599071416, 13.74590378743879882 ) ) ;
#3559 = EDGE_CURVE ( 'NONE', #10410, #17454, #21374, .T. ) ;
#3560 = DIRECTION ( 'NONE',  ( 0.000000000000000000, 0.000000000000000000, -1.000000000000000000 ) ) ;
#3561 = EDGE_CURVE ( 'NONE', #3486, #14859, #9988, .T. ) ;
#3562 = CARTESIAN_POINT ( 'NONE',  ( -31.63662752439705272, 0.000000000000000000, -18.50000000000000000 ) ) ;
#3563 = DIRECTION ( 'NONE',  ( 0.000000000000000000, 0.000000000000000000, 1.000000000000000000 ) ) ;
#3564 = ORIENTED_EDGE ( 'NONE', *, *, #8385, .T. ) ;
#3565 = CARTESIAN_POINT ( 'NONE',  ( 23.26572410265648116, 3.298136152264957932, 13.49420500573775428 ) ) ;
#3566 = CARTESIAN_POINT ( 'NONE',  ( -1.824728116533986810, 43.26054587065083012, 37.66679706732590915 ) ) ;
#3567 = CARTESIAN_POINT ( 'NONE',  ( 14.96174975910705918, 32.10873716947361345, 13.05380965755522737 ) ) ;
#3568 = CARTESIAN_POINT ( 'NONE',  ( -1.724728116533986721, 42.36054587065083155, 35.70876104995653577 ) ) ;
#3569 = EDGE_LOOP ( 'NONE', ( #2432, #14583, #6590, #21609 ) ) ;
#3570 = CARTESIAN_POINT ( 'NONE',  ( -9.178906393579158163, 42.46645089659918426, 68.06527860057354928 ) ) ;
#3571 = CIRCLE ( 'NONE', #3214, 0.04999999999999991257 ) ;
#3572 = CARTESIAN_POINT ( 'NONE',  ( -15.95292532278785913, 34.11873716947361856, 68.00000000000000000 ) ) ;
#3573 = ORIENTED_EDGE ( 'NONE', *, *, #3348, .T. ) ;
#3574 = DIRECTION ( 'NONE',  ( 1.000000000000000000, 0.000000000000000000, 0.000000000000000000 ) ) ;
#3575 = CARTESIAN_POINT ( 'NONE',  ( -29.37540678000427619, 6.000000000000000000, 7.500000000000000000 ) ) ;
#3576 = ORIENTED_EDGE ( 'NONE', *, *, #14050, .T. ) ;
#3577 = ORIENTED_EDGE ( 'NONE', *, *, #4685, .T. ) ;
#3578 = DIRECTION ( 'NONE',  ( 0.000000000000000000, 0.000000000000000000, 1.000000000000000000 ) ) ;
#3579 = ORIENTED_EDGE ( 'NONE', *, *, #4705, .T. ) ;
#3580 = EDGE_CURVE ( 'NONE', #11507, #1591, #19454, .T. ) ;
#3581 = CARTESIAN_POINT ( 'NONE',  ( 0.000000000000000000, 42.31054587065082728, 35.75876104995654003 ) ) ;
#3582 = AXIS2_PLACEMENT_3D ( 'NONE', #21698, #12604, #3107 ) ;
#3583 = ORIENTED_EDGE ( 'NONE', *, *, #21569, .F. ) ;
#3584 = DIRECTION ( 'NONE',  ( 2.832483164223434527E-16, 1.000000000000000000, 0.000000000000000000 ) ) ;
#3585 = CIRCLE ( 'NONE', #10737, 2.299999999999993161 ) ;
#3586 = TOROIDAL_SURFACE ( 'NONE', #16062, 2.274596669241483848, 0.2999999999999999889 ) ;
#3587 = ADVANCED_FACE ( 'NONE', ( #17991 ), #12717, .T. ) ;
#3588 = CARTESIAN_POINT ( 'NONE',  ( 15.95292532278785913, 52.11873716947361856, 13.99999999999999822 ) ) ;
#3589 = FACE_OUTER_BOUND ( 'NONE', #14175, .T. ) ;
#3590 = CARTESIAN_POINT ( 'NONE',  ( 1.824728116533979705, 42.36054587065083155, 33.66679706732590915 ) ) ;
#3591 = LINE ( 'NONE', #15100, #2486 ) ;
#3592 = CARTESIAN_POINT ( 'NONE',  ( 0.000000000000000000, 5.299999999999999822, 7.200000000000000178 ) ) ;
#3593 = DIRECTION ( 'NONE',  ( 1.000000000000000000, 0.000000000000000000, 0.000000000000000000 ) ) ;
#3594 = VECTOR ( 'NONE', #16206, 1000.000000000000000 ) ;
#3595 = EDGE_LOOP ( 'NONE', ( #12234, #11194, #15690, #14804 ) ) ;
#3596 = DIRECTION ( 'NONE',  ( -0.000000000000000000, -0.000000000000000000, -1.000000000000000000 ) ) ;
#3597 = CYLINDRICAL_SURFACE ( 'NONE', #9198, 0.2999999999999999334 ) ;
#3598 = CIRCLE ( 'NONE', #16791, 0.2500000000000011657 ) ;
#3599 = PRODUCT_DEFINITION_SHAPE ( 'NONE', 'NONE',  #22175 ) ;
#3600 = EDGE_CURVE ( 'NONE', #13259, #12460, #11063, .T. ) ;
#3601 = ORIENTED_EDGE ( 'NONE', *, *, #13761, .T. ) ;
#3602 = ORIENTED_EDGE ( 'NONE', *, *, #3561, .T. ) ;
#3603 = CARTESIAN_POINT ( 'NONE',  ( -30.07540678000427548, -63.74634676501045050, 7.500000000000000000 ) ) ;
#3604 = VERTEX_POINT ( 'NONE', #16434 ) ;
#3605 = EDGE_LOOP ( 'NONE', ( #8555, #15272, #13455, #14938 ) ) ;
#3606 = EDGE_CURVE ( 'NONE', #3489, #6504, #7710, .T. ) ;
#3607 = CARTESIAN_POINT ( 'NONE',  ( 1.724728116533979838, 42.36054587065083155, 49.66679706732590915 ) ) ;
#3608 = EDGE_LOOP ( 'NONE', ( #17508, #17437, #13832, #1955 ) ) ;
#3609 = ORIENTED_EDGE ( 'NONE', *, *, #13336, .T. ) ;
#3610 = AXIS2_PLACEMENT_3D ( 'NONE', #14941, #11475, #1172 ) ;
#3611 = CYLINDRICAL_SURFACE ( 'NONE', #19496, 0.2999999999999999334 ) ;
#3612 = FACE_OUTER_BOUND ( 'NONE', #3123, .T. ) ;
#3613 = CIRCLE ( 'NONE', #5039, 0.6000000000000033085 ) ;
#3614 = CARTESIAN_POINT ( 'NONE',  ( 23.02398829872514341, 2.501746539338821851, 13.57884938331724278 ) ) ;
#3615 = DIRECTION ( 'NONE',  ( 0.000000000000000000, -1.000000000000000000, -0.000000000000000000 ) ) ;
#3616 = DIRECTION ( 'NONE',  ( 0.000000000000000000, -0.000000000000000000, -1.000000000000000000 ) ) ;
#3617 = FACE_OUTER_BOUND ( 'NONE', #18202, .T. ) ;
#3618 = FACE_OUTER_BOUND ( 'NONE', #12563, .T. ) ;
#3619 = DIRECTION ( 'NONE',  ( 0.000000000000000000, 0.000000000000000000, 1.000000000000000000 ) ) ;
#3620 = EDGE_CURVE ( 'NONE', #19432, #5550, #16838, .T. ) ;
#3621 = FACE_OUTER_BOUND ( 'NONE', #2135, .T. ) ;
#3622 = AXIS2_PLACEMENT_3D ( 'NONE', #14975, #13601, #3006 ) ;
#3623 = EDGE_LOOP ( 'NONE', ( #16917, #15224, #16249, #4298 ) ) ;
#3624 = ORIENTED_EDGE ( 'NONE', *, *, #15709, .T. ) ;
#3625 = CARTESIAN_POINT ( 'NONE',  ( 14.66174975910705847, 42.11054587065083155, 13.50000000000000000 ) ) ;
#3626 = DIRECTION ( 'NONE',  ( 1.000000000000000000, 0.000000000000000000, 0.000000000000000000 ) ) ;
#3627 = EDGE_LOOP ( 'NONE', ( #5733, #10876, #5316, #3452 ) ) ;
#3628 = TOROIDAL_SURFACE ( 'NONE', #1451, 0.05000000000000000278, 0.05000000000000000278 ) ;
#3629 = EDGE_CURVE ( 'NONE', #513, #10751, #3555, .T. ) ;
#3630 = VECTOR ( 'NONE', #7552, 1000.000000000000000 ) ;
#3631 = ADVANCED_FACE ( 'NONE', ( #4128 ), #2665, .T. ) ;
#3632 = DIRECTION ( 'NONE',  ( 1.000000000000000000, 0.000000000000000000, 0.000000000000000000 ) ) ;
#3633 = VECTOR ( 'NONE', #21041, 1000.000000000000000 ) ;
#3634 = ADVANCED_FACE ( 'NONE', ( #6164 ), #4248, .T. ) ;
#3635 = CIRCLE ( 'NONE', #16112, 0.09999999999999939493 ) ;
#3636 = DIRECTION ( 'NONE',  ( 1.000000000000000000, 0.000000000000000000, 0.000000000000000000 ) ) ;
#3637 = CARTESIAN_POINT ( 'NONE',  ( 17.93704824106378837, 0.000000000000000000, 13.87500000000000000 ) ) ;
#3638 = ORIENTED_EDGE ( 'NONE', *, *, #14725, .F. ) ;
#3639 = FACE_OUTER_BOUND ( 'NONE', #3914, .T. ) ;
#3640 = CYLINDRICAL_SURFACE ( 'NONE', #320, 0.2999999999999999334 ) ;
#3641 = DIRECTION ( 'NONE',  ( 1.000000000000000000, -0.000000000000000000, -0.000000000000000000 ) ) ;
#3642 = DIRECTION ( 'NONE',  ( -1.000000000000000000, 0.000000000000000000, 0.000000000000000000 ) ) ;
#3643 = DIRECTION ( 'NONE',  ( 0.000000000000000000, 0.000000000000000000, -1.000000000000000000 ) ) ;
#3644 = LINE ( 'NONE', #14123, #16996 ) ;
#3645 = CARTESIAN_POINT ( 'NONE',  ( -1.836970198721029934E-16, 72.00000000000001421, 1.800000000000000044 ) ) ;
#3646 = ADVANCED_FACE ( 'NONE', ( #17772 ), #2473, .T. ) ;
#3647 = EDGE_LOOP ( 'NONE', ( #19238, #7391, #2907, #1058 ) ) ;
#3648 = CARTESIAN_POINT ( 'NONE',  ( -1.774728116533986544, 43.31054587065082728, 39.80876104995653719 ) ) ;
#3649 = CARTESIAN_POINT ( 'NONE',  ( -15.95292532278785913, -34.11873716947361856, 68.00000000000000000 ) ) ;
#3650 = CARTESIAN_POINT ( 'NONE',  ( -1.774728116533986766, 42.31054587065082728, 29.66679706732590560 ) ) ;
#3651 = VERTEX_POINT ( 'NONE', #14407 ) ;
#3652 = ORIENTED_EDGE ( 'NONE', *, *, #19586, .T. ) ;
#3653 = CARTESIAN_POINT ( 'NONE',  ( -29.13662752439705272, 0.000000000000000000, 13.50000000000000000 ) ) ;
#3654 = DIRECTION ( 'NONE',  ( 0.000000000000000000, 1.000000000000000000, 0.000000000000000000 ) ) ;
#3655 = CIRCLE ( 'NONE', #5806, 5.193574995607838751 ) ;
#3656 = CARTESIAN_POINT ( 'NONE',  ( 29.13662752439705272, 0.000000000000000000, 3.500000000000000000 ) ) ;
#3657 = CIRCLE ( 'NONE', #2576, 4.051418481279139172 ) ;
#3658 = CIRCLE ( 'NONE', #11500, 0.6999999999999992895 ) ;
#3659 = DIRECTION ( 'NONE',  ( -0.000000000000000000, -0.000000000000000000, -1.000000000000000000 ) ) ;
#3660 = EDGE_CURVE ( 'NONE', #879, #18072, #20710, .T. ) ;
#3661 = ORIENTED_EDGE ( 'NONE', *, *, #18724, .F. ) ;
#3662 = CARTESIAN_POINT ( 'NONE',  ( -25.37540678000427263, -66.94634676501046044, 13.19999999999999929 ) ) ;
#3663 = EDGE_CURVE ( 'NONE', #19429, #20933, #6780, .T. ) ;
#3664 = EDGE_LOOP ( 'NONE', ( #14267, #9014, #13412, #14288, #10618, #3638 ) ) ;
#3665 = LINE ( 'NONE', #13503, #13123 ) ;
#3666 = LINE ( 'NONE', #1763, #18150 ) ;
#3667 = DIRECTION ( 'NONE',  ( 0.000000000000000000, 0.000000000000000000, 1.000000000000000000 ) ) ;
#3668 = CARTESIAN_POINT ( 'NONE',  ( 1.774728116533973665, 42.31054587065082728, -3.739806423751037426E-16 ) ) ;
#3669 = ORIENTED_EDGE ( 'NONE', *, *, #12333, .T. ) ;
#3670 = CARTESIAN_POINT ( 'NONE',  ( 23.32398829872514057, 3.528912754968628995, 13.50000000000000178 ) ) ;
#3671 = FACE_OUTER_BOUND ( 'NONE', #20180, .T. ) ;
#3672 = CIRCLE ( 'NONE', #16143, 0.05000000000000143219 ) ;
#3673 = CIRCLE ( 'NONE', #9743, 0.04999999999999991257 ) ;
#3674 = CARTESIAN_POINT ( 'NONE',  ( -15.21174975910705207, 42.31054587065082728, 68.50000000000000000 ) ) ;
#3675 = CARTESIAN_POINT ( 'NONE',  ( 31.50000000000002132, -71.70000000000001705, 1.500000000000000000 ) ) ;
#3676 = ORIENTED_EDGE ( 'NONE', *, *, #12398, .T. ) ;
#3677 = CARTESIAN_POINT ( 'NONE',  ( -9.178906393579161715, 44.96645089659919137, 61.53912392244307483 ) ) ;
#3678 = VERTEX_POINT ( 'NONE', #2783 ) ;
#3679 = DIRECTION ( 'NONE',  ( -1.000000000000000000, 0.000000000000000000, 0.000000000000000000 ) ) ;
#3680 = VERTEX_POINT ( 'NONE', #2563 ) ;
#3681 = CIRCLE ( 'NONE', #1881, 0.05000000000000143219 ) ;
#3682 = CARTESIAN_POINT ( 'NONE',  ( 0.000000000000000000, 5.299999999999999822, 7.200000000000000178 ) ) ;
#3683 = EDGE_CURVE ( 'NONE', #5528, #14977, #21602, .T. ) ;
#3684 = FACE_OUTER_BOUND ( 'NONE', #12824, .T. ) ;
#3685 = ORIENTED_EDGE ( 'NONE', *, *, #10122, .T. ) ;
#3686 = ORIENTED_EDGE ( 'NONE', *, *, #8950, .F. ) ;
#3687 = EDGE_CURVE ( 'NONE', #8963, #11507, #324, .T. ) ;
#3688 = ORIENTED_EDGE ( 'NONE', *, *, #680, .T. ) ;
#3689 = CARTESIAN_POINT ( 'NONE',  ( -29.50000000000002842, 2.473451120191013874, 0.2503166595423103602 ) ) ;
#3690 = CARTESIAN_POINT ( 'NONE',  ( 34.39999999999998437, -85.00000000000000000, 0.3000000000000042077 ) ) ;
#3691 = CARTESIAN_POINT ( 'NONE',  ( -1.724728116533986721, 43.26054587065083012, 29.66679706732590560 ) ) ;
#3692 = CARTESIAN_POINT ( 'NONE',  ( -1.724728116533986721, 42.36054587065083155, 29.76679706732590702 ) ) ;
#3693 = ORIENTED_EDGE ( 'NONE', *, *, #5591, .F. ) ;
#3694 = CARTESIAN_POINT ( 'NONE',  ( 34.39999999999998437, 85.00000000000000000, 0.3000000000000042077 ) ) ;
#3695 = DIRECTION ( 'NONE',  ( -1.000000000000000000, 0.000000000000000000, 0.000000000000000000 ) ) ;
#3696 = DIRECTION ( 'NONE',  ( -1.000000000000000000, 0.000000000000000000, 0.000000000000000000 ) ) ;
#3697 = VERTEX_POINT ( 'NONE', #18227 ) ;
#3698 = EDGE_CURVE ( 'NONE', #22, #16620, #19268, .T. ) ;
#3699 = FACE_OUTER_BOUND ( 'NONE', #11269, .T. ) ;
#3700 = CARTESIAN_POINT ( 'NONE',  ( -14.96174975910705207, 51.76873716947361714, 13.79999999999999893 ) ) ;
#3701 = EDGE_CURVE ( 'NONE', #9271, #3754, #21051, .T. ) ;
#3702 = ORIENTED_EDGE ( 'NONE', *, *, #13744, .F. ) ;
#3703 = ORIENTED_EDGE ( 'NONE', *, *, #2659, .T. ) ;
#3704 = FACE_OUTER_BOUND ( 'NONE', #17459, .T. ) ;
#3705 = DIRECTION ( 'NONE',  ( 0.9219482411244461773, 0.3873131042032275095, 0.000000000000000000 ) ) ;
#3706 = EDGE_LOOP ( 'NONE', ( #10172, #5589, #16180, #13343 ) ) ;
#3707 =( GEOMETRIC_REPRESENTATION_CONTEXT ( 3 ) GLOBAL_UNCERTAINTY_ASSIGNED_CONTEXT ( ( #12276 ) ) GLOBAL_UNIT_ASSIGNED_CONTEXT ( ( #2697, #20958, #10986 ) ) REPRESENTATION_CONTEXT ( 'NONE', 'WORKASPACE' ) );
#3708 = CARTESIAN_POINT ( 'NONE',  ( 23.20982120895258660, -3.064530420494568475, 13.47289532992770233 ) ) ;
#3709 = ORIENTED_EDGE ( 'NONE', *, *, #11363, .T. ) ;
#3710 = ORIENTED_EDGE ( 'NONE', *, *, #11319, .F. ) ;
#3711 = DIRECTION ( 'NONE',  ( -1.000000000000000000, 0.000000000000000000, 0.000000000000000000 ) ) ;
#3712 = CARTESIAN_POINT ( 'NONE',  ( 31.50000000000002132, 71.00000000000001421, 1.800000000000000044 ) ) ;
#3713 = AXIS2_PLACEMENT_3D ( 'NONE', #15511, #297, #1875 ) ;
#3714 = CARTESIAN_POINT ( 'NONE',  ( -28.87540678000427619, 0.000000000000000000, 7.799999999999999822 ) ) ;
#3715 = ADVANCED_FACE ( 'NONE', ( #18744 ), #7829, .T. ) ;
#3716 = CARTESIAN_POINT ( 'NONE',  ( 33.79999999999999716, -85.00000000000000000, 2.931682674400803201E-15 ) ) ;
#3717 = SURFACE_SIDE_STYLE ('',( #453 ) ) ;
#3718 = PLANE ( 'NONE',  #16152 ) ;
#3719 = AXIS2_PLACEMENT_3D ( 'NONE', #6960, #20258, #3360 ) ;
#3720 = PLANE ( 'NONE',  #8657 ) ;
#3721 = PRODUCT_DEFINITION_FORMATION_WITH_SPECIFIED_SOURCE ( 'ANY', '', #1228, .NOT_KNOWN. ) ;
#3722 = CARTESIAN_POINT ( 'NONE',  ( 23.07462249345254790, -2.431574673422045141, 13.33584746657814080 ) ) ;
#3723 = CARTESIAN_POINT ( 'NONE',  ( 14.75227361591076480, -52.14371094704548426, 13.49999999999999467 ) ) ;
#3724 = AXIS2_PLACEMENT_3D ( 'NONE', #20435, #4660, #3308 ) ;
#3725 = EDGE_CURVE ( 'NONE', #21935, #21679, #2257, .T. ) ;
#3726 = DIRECTION ( 'NONE',  ( 0.000000000000000000, 0.000000000000000000, 1.000000000000000000 ) ) ;
#3727 = EDGE_CURVE ( 'NONE', #12867, #1401, #17813, .T. ) ;
#3728 = CARTESIAN_POINT ( 'NONE',  ( -3.127054932750481964, 32.61873716947361856, 68.00000000000000000 ) ) ;
#3729 = VERTEX_POINT ( 'NONE', #7421 ) ;
#3730 = EDGE_LOOP ( 'NONE', ( #8356, #5401, #4211, #6254 ) ) ;
#3731 = DIRECTION ( 'NONE',  ( 0.000000000000000000, 1.000000000000000000, 0.000000000000000000 ) ) ;
#3732 = CARTESIAN_POINT ( 'NONE',  ( -1.724728116533986721, 42.36054587065083155, 49.66679706732590915 ) ) ;
#3733 = ORIENTED_EDGE ( 'NONE', *, *, #925, .F. ) ;
#3734 = ORIENTED_EDGE ( 'NONE', *, *, #3909, .T. ) ;
#3735 = ADVANCED_FACE ( 'NONE', ( #18230 ), #18541, .F. ) ;
#3736 = DIRECTION ( 'NONE',  ( 0.000000000000000000, 0.000000000000000000, -1.000000000000000000 ) ) ;
#3737 = CARTESIAN_POINT ( 'NONE',  ( -30.37540678000427619, -63.74634676501045050, 7.500000000000000000 ) ) ;
#3738 = ORIENTED_EDGE ( 'NONE', *, *, #7498, .F. ) ;
#3739 = DIRECTION ( 'NONE',  ( -1.000000000000000000, -0.000000000000000000, -0.000000000000000000 ) ) ;
#3740 = DIRECTION ( 'NONE',  ( 1.000000000000000000, 0.000000000000000000, 0.000000000000000000 ) ) ;
#3741 = DIRECTION ( 'NONE',  ( 1.000000000000000000, 7.973140176887192922E-16, 0.000000000000000000 ) ) ;
#3742 = CARTESIAN_POINT ( 'NONE',  ( 1.724728116533978728, 43.31054587065082728, 29.71679706732590631 ) ) ;
#3743 = CARTESIAN_POINT ( 'NONE',  ( -1.824728116533986810, 42.36054587065083155, 43.80876104995653719 ) ) ;
#3744 = CARTESIAN_POINT ( 'NONE',  ( 1.774728116533979438, 42.31054587065082728, 35.80876104995653009 ) ) ;
#3745 = ADVANCED_FACE ( 'NONE', ( #11065 ), #16087, .T. ) ;
#3746 = EDGE_CURVE ( 'NONE', #19066, #11236, #989, .T. ) ;
#3747 = CARTESIAN_POINT ( 'NONE',  ( 25.37540678000426908, 36.74634676501047181, 13.79999999999999893 ) ) ;
#3748 = DIRECTION ( 'NONE',  ( 0.000000000000000000, 1.000000000000000000, 0.000000000000000000 ) ) ;
#3749 = ADVANCED_FACE ( 'NONE', ( #1104 ), #14753, .F. ) ;
#3750 = LINE ( 'NONE', #17507, #8481 ) ;
#3751 = ORIENTED_EDGE ( 'NONE', *, *, #11193, .T. ) ;
#3752 = AXIS2_PLACEMENT_3D ( 'NONE', #1342, #8299, #8195 ) ;
#3753 = AXIS2_PLACEMENT_3D ( 'NONE', #12635, #1015, #19601 ) ;
#3754 = VERTEX_POINT ( 'NONE', #7845 ) ;
#3755 = CARTESIAN_POINT ( 'NONE',  ( 27.75399754406947750, -2.121775353753131643, 0.1432465332877360387 ) ) ;
#3756 = CARTESIAN_POINT ( 'NONE',  ( 14.96174975910705918, 51.86873716947361856, 13.05380965755522737 ) ) ;
#3757 = FACE_OUTER_BOUND ( 'NONE', #6833, .T. ) ;
#3758 = FACE_BOUND ( 'NONE', #17109, .T. ) ;
#3759 = ORIENTED_EDGE ( 'NONE', *, *, #3271, .F. ) ;
#3760 = CARTESIAN_POINT ( 'NONE',  ( 1.774728116533979660, 43.26054587065083012, 27.80876104995653719 ) ) ;
#3761 = ADVANCED_FACE ( 'NONE', ( #19918 ), #7715, .T. ) ;
#3762 = ORIENTED_EDGE ( 'NONE', *, *, #7767, .T. ) ;
#3763 = CARTESIAN_POINT ( 'NONE',  ( 31.50000000000002132, 71.70000000000001705, 1.500000000000000000 ) ) ;
#3764 = DIRECTION ( 'NONE',  ( 0.000000000000000000, 0.000000000000000000, 1.000000000000000000 ) ) ;
#3765 = VECTOR ( 'NONE', #1399, 1000.000000000000000 ) ;
#3766 = CYLINDRICAL_SURFACE ( 'NONE', #12197, 0.5000000000000004441 ) ;
#3767 = CIRCLE ( 'NONE', #5199, 1.299999999999999156 ) ;
#3768 = CARTESIAN_POINT ( 'NONE',  ( 29.13662752439705272, 0.000000000000000000, 13.19999999999999929 ) ) ;
#3769 = ORIENTED_EDGE ( 'NONE', *, *, #14736, .T. ) ;
#3770 = CARTESIAN_POINT ( 'NONE',  ( 23.13120573414546399, 2.711843391866131103, 13.41529098820777222 ) ) ;
#3771 = CARTESIAN_POINT ( 'NONE',  ( -1.824728116533986810, 43.31054587065082728, 31.70876104995653932 ) ) ;
#3772 = DIRECTION ( 'NONE',  ( 0.000000000000000000, 0.000000000000000000, 1.000000000000000000 ) ) ;
#3773 = DIRECTION ( 'NONE',  ( 0.000000000000000000, 0.000000000000000000, 1.000000000000000000 ) ) ;
#3774 = ORIENTED_EDGE ( 'NONE', *, *, #14689, .T. ) ;
#3775 = CARTESIAN_POINT ( 'NONE',  ( 17.45292532278785913, 0.000000000000000000, 14.00000000000000000 ) ) ;
#3776 = EDGE_CURVE ( 'NONE', #7580, #13533, #18105, .T. ) ;
#3777 = ORIENTED_EDGE ( 'NONE', *, *, #10168, .T. ) ;
#3778 = CARTESIAN_POINT ( 'NONE',  ( 34.69999999999998863, -84.70000000000001705, 79.39999999999999147 ) ) ;
#3779 = EDGE_CURVE ( 'NONE', #12641, #21318, #21770, .T. ) ;
#3780 = DIRECTION ( 'NONE',  ( -0.000000000000000000, -0.000000000000000000, 1.000000000000000000 ) ) ;
#3781 = ORIENTED_EDGE ( 'NONE', *, *, #10455, .F. ) ;
#3782 = CIRCLE ( 'NONE', #15543, 0.2999999999999999334 ) ;
#3783 = VERTEX_POINT ( 'NONE', #16536 ) ;
#3785 = EDGE_CURVE ( 'NONE', #7349, #16038, #17993, .T. ) ;
#3784 = DIRECTION ( 'NONE',  ( -1.000000000000000000, 0.000000000000000000, 0.000000000000000000 ) ) ;
#3786 = CARTESIAN_POINT ( 'NONE',  ( -18.91037735075775217, 42.46645089659918426, 13.74999999999999822 ) ) ;
#3787 = ORIENTED_EDGE ( 'NONE', *, *, #100, .F. ) ;
#3788 = VECTOR ( 'NONE', #11219, 1000.000000000000000 ) ;
#3789 = ORIENTED_EDGE ( 'NONE', *, *, #15261, .T. ) ;
#3790 = AXIS2_PLACEMENT_3D ( 'NONE', #3311, #8579, #3414 ) ;
#3791 = CIRCLE ( 'NONE', #21298, 0.3000000000000003775 ) ;
#3792 = ORIENTED_EDGE ( 'NONE', *, *, #9151, .F. ) ;
#3793 = ADVANCED_FACE ( 'NONE', ( #12840 ), #2667, .F. ) ;
#3794 = EDGE_LOOP ( 'NONE', ( #9587, #437, #16232, #20032 ) ) ;
#3795 = DIRECTION ( 'NONE',  ( 1.000000000000000000, -0.000000000000000000, -0.000000000000000000 ) ) ;
#3796 = CIRCLE ( 'NONE', #7038, 0.5000000000000004441 ) ;
#3797 = AXIS2_PLACEMENT_3D ( 'NONE', #20694, #3679, #15516 ) ;
#3798 = CARTESIAN_POINT ( 'NONE',  ( 1.724728116533979838, 43.31054587065082728, 53.66679706732590915 ) ) ;
#3799 = AXIS2_PLACEMENT_3D ( 'NONE', #18597, #6873, #3276 ) ;
#3800 = CARTESIAN_POINT ( 'NONE',  ( 29.01868551570922605, 6.499165645473476971, 7.532495484408729958 ) ) ;
#3801 = CYLINDRICAL_SURFACE ( 'NONE', #16725, 0.5000000000000004441 ) ;
#3802 = ADVANCED_FACE ( 'NONE', ( #20033 ), #14855, .T. ) ;
#3803 = PRODUCT_DEFINITION_CONTEXT ( 'detailed design', #12566, 'design' ) ;
#3804 = ORIENTED_EDGE ( 'NONE', *, *, #637, .T. ) ;
#3805 = CARTESIAN_POINT ( 'NONE',  ( 26.37540678000427619, 10.94079601157914539, 13.79999999999999893 ) ) ;
#3806 = CIRCLE ( 'NONE', #19234, 0.05000000000000143219 ) ;
#3807 = VECTOR ( 'NONE', #15902, 1000.000000000000000 ) ;
#3808 = DIRECTION ( 'NONE',  ( -1.000000000000000000, 0.000000000000000000, 0.000000000000000000 ) ) ;
#3809 = LINE ( 'NONE', #2334, #4737 ) ;
#3810 = ADVANCED_FACE ( 'NONE', ( #9954 ), #10167, .F. ) ;
#3811 = ORIENTED_EDGE ( 'NONE', *, *, #3915, .T. ) ;
#3812 = CARTESIAN_POINT ( 'NONE',  ( -23.32398829872514057, 5.683640910026983128, 13.79999999999999893 ) ) ;
#3813 = DIRECTION ( 'NONE',  ( 0.000000000000000000, 0.000000000000000000, 1.000000000000000000 ) ) ;
#3814 = ORIENTED_EDGE ( 'NONE', *, *, #11445, .T. ) ;
#3815 = AXIS2_PLACEMENT_3D ( 'NONE', #4422, #19763, #9798 ) ;
#3816 = CIRCLE ( 'NONE', #13805, 0.2999999999999999334 ) ;
#3817 = ORIENTED_EDGE ( 'NONE', *, *, #2205, .F. ) ;
#3818 = TOROIDAL_SURFACE ( 'NONE', #1289, 1.500000000000000000, 0.5000000000000000000 ) ;
#3819 = DIRECTION ( 'NONE',  ( 0.000000000000000000, 1.000000000000000000, 0.000000000000000000 ) ) ;
#3820 = ORIENTED_EDGE ( 'NONE', *, *, #9878, .T. ) ;
#3821 = AXIS2_PLACEMENT_3D ( 'NONE', #9862, #15212, #21851 ) ;
#3822 = CARTESIAN_POINT ( 'NONE',  ( 23.02398829872514341, -2.157133714763071364, 13.26827027136048720 ) ) ;
#3823 = ORIENTED_EDGE ( 'NONE', *, *, #20888, .F. ) ;
#3824 = VERTEX_POINT ( 'NONE', #21930 ) ;
#3825 = DIRECTION ( 'NONE',  ( -0.000000000000000000, -0.000000000000000000, -1.000000000000000000 ) ) ;
#3826 = EDGE_CURVE ( 'NONE', #11974, #1033, #11727, .T. ) ;
#3827 = CARTESIAN_POINT ( 'NONE',  ( 1.824728116533979261, 43.26054587065083012, 39.80876104995653719 ) ) ;
#3828 = DIRECTION ( 'NONE',  ( -1.000000000000000000, 0.000000000000000000, 0.000000000000000000 ) ) ;
#3829 = CIRCLE ( 'NONE', #21714, 0.5000000000000004441 ) ;
#3830 = EDGE_CURVE ( 'NONE', #119, #16405, #14587, .T. ) ;
#3831 = EDGE_CURVE ( 'NONE', #18, #15927, #13401, .T. ) ;
#3832 = VECTOR ( 'NONE', #3070, 1000.000000000000000 ) ;
#3833 = CIRCLE ( 'NONE', #5631, 0.5999999999999998668 ) ;
#3834 = CIRCLE ( 'NONE', #16667, 1.750000000000001554 ) ;
#3835 = DIRECTION ( 'NONE',  ( 0.000000000000000000, 0.000000000000000000, 1.000000000000000000 ) ) ;
#3836 = AXIS2_PLACEMENT_3D ( 'NONE', #20818, #7277, #14076 ) ;
#3837 = DIRECTION ( 'NONE',  ( 1.000000000000000000, -1.094601647044990554E-16, 0.000000000000000000 ) ) ;
#3838 = DIRECTION ( 'NONE',  ( -4.336808689941893885E-15, 0.000000000000000000, 1.000000000000000000 ) ) ;
#3839 = CARTESIAN_POINT ( 'NONE',  ( 1.724728116533979616, 43.31054587065082728, 47.70876104995654288 ) ) ;
#3840 = CARTESIAN_POINT ( 'NONE',  ( -29.17540678000427690, 0.000000000000000000, 7.799999999999999822 ) ) ;
#3841 = CARTESIAN_POINT ( 'NONE',  ( -15.05282292896044005, -52.05812657117054698, 13.87232935072191964 ) ) ;
#3842 = VERTEX_POINT ( 'NONE', #3121 ) ;
#3843 = ORIENTED_EDGE ( 'NONE', *, *, #20782, .F. ) ;
#3844 = DIRECTION ( 'NONE',  ( -0.000000000000000000, -0.000000000000000000, 1.000000000000000000 ) ) ;
#3845 = CARTESIAN_POINT ( 'NONE',  ( 4.127054932750481520, 32.93424481021354921, 68.00000000000000000 ) ) ;
#3846 = EDGE_LOOP ( 'NONE', ( #2048, #8028, #20970 ) ) ;
#3847 = EDGE_CURVE ( 'NONE', #5475, #10300, #312, .T. ) ;
#3848 = VECTOR ( 'NONE', #17551, 1000.000000000000000 ) ;
#3849 = CIRCLE ( 'NONE', #7429, 0.2999999999999999889 ) ;
#3850 = ORIENTED_EDGE ( 'NONE', *, *, #4592, .F. ) ;
#3851 = AXIS2_PLACEMENT_3D ( 'NONE', #1411, #3216, #21911 ) ;
#3852 = VECTOR ( 'NONE', #20774, 1000.000000000000000 ) ;
#3853 = AXIS2_PLACEMENT_3D ( 'NONE', #7641, #5226, #12135 ) ;
#3854 = ADVANCED_FACE ( 'NONE', ( #6501 ), #18667, .F. ) ;
#3855 = CARTESIAN_POINT ( 'NONE',  ( -21.92816239687475743, 42.46645089659918426, 13.74999999999999822 ) ) ;
#3856 = CARTESIAN_POINT ( 'NONE',  ( 34.99999999999999289, 85.00000000000000000, 0.6000000000000033085 ) ) ;
#3857 = EDGE_LOOP ( 'NONE', ( #21273, #18853, #9256, #9124 ) ) ;
#3858 = DIRECTION ( 'NONE',  ( 1.000000000000000000, -0.000000000000000000, 0.000000000000000000 ) ) ;
#3859 = CARTESIAN_POINT ( 'NONE',  ( -1.824728116533986810, 42.36054587065083155, 43.70876104995653577 ) ) ;
#3860 = CARTESIAN_POINT ( 'NONE',  ( -31.50000000000002132, -71.70000000000001705, 1.800000000000000044 ) ) ;
#3861 = FACE_OUTER_BOUND ( 'NONE', #15919, .T. ) ;
#3862 = CARTESIAN_POINT ( 'NONE',  ( -33.20000000000000284, 85.00000000000000000, 1.800000000000000266 ) ) ;
#3863 = AXIS2_PLACEMENT_3D ( 'NONE', #7830, #8259, #3101 ) ;
#3864 = AXIS2_PLACEMENT_3D ( 'NONE', #7246, #19205, #7139 ) ;
#3865 = VECTOR ( 'NONE', #11253, 1000.000000000000000 ) ;
#3866 = DIRECTION ( 'NONE',  ( 1.000000000000000000, 0.000000000000000000, 0.000000000000000000 ) ) ;
#3867 = DIRECTION ( 'NONE',  ( -1.000000000000000000, 0.000000000000000000, 0.000000000000000000 ) ) ;
#3868 = ORIENTED_EDGE ( 'NONE', *, *, #21691, .F. ) ;
#3869 = CARTESIAN_POINT ( 'NONE',  ( -17.95292532278785913, -38.74634676501045760, 109.6002446535588319 ) ) ;
#3870 = CARTESIAN_POINT ( 'NONE',  ( -31.50000000000002132, 71.00000000000001421, 3.200000000000000178 ) ) ;
#3871 = CIRCLE ( 'NONE', #11360, 4.193574995607837863 ) ;
#3872 = CARTESIAN_POINT ( 'NONE',  ( -4.127054932750482408, 32.93424481021354921, 68.50000000000000000 ) ) ;
#3873 = EDGE_LOOP ( 'NONE', ( #4239, #18841, #20135, #8926 ) ) ;
#3874 = VECTOR ( 'NONE', #2489, 1000.000000000000000 ) ;
#3875 = ORIENTED_EDGE ( 'NONE', *, *, #14973, .T. ) ;
#3876 = CARTESIAN_POINT ( 'NONE',  ( 26.61833302554978786, -9.663695060508651125, 13.50000000000000000 ) ) ;
#3877 = DIRECTION ( 'NONE',  ( -1.000000000000000000, 0.000000000000000000, 0.000000000000000000 ) ) ;
#3878 = AXIS2_PLACEMENT_3D ( 'NONE', #6966, #8742, #215 ) ;
#3879 = CARTESIAN_POINT ( 'NONE',  ( -23.83662752439705201, 0.000000000000000000, 7.200000000000000178 ) ) ;
#3880 = ORIENTED_EDGE ( 'NONE', *, *, #12416, .F. ) ;
#3881 = FACE_OUTER_BOUND ( 'NONE', #3423, .T. ) ;
#3882 = EDGE_LOOP ( 'NONE', ( #8952, #17672, #4314, #13954, #3868 ) ) ;
#3883 = DIRECTION ( 'NONE',  ( 0.000000000000000000, -0.000000000000000000, -1.000000000000000000 ) ) ;
#3884 = AXIS2_PLACEMENT_3D ( 'NONE', #467, #15901, #4065 ) ;
#3885 = AXIS2_PLACEMENT_3D ( 'NONE', #21490, #21597, #10059 ) ;
#3886 = ADVANCED_FACE ( 'NONE', ( #20578 ), #20136, .F. ) ;
#3887 = EDGE_LOOP ( 'NONE', ( #13715, #243, #12699, #7282 ) ) ;
#3888 = ADVANCED_FACE ( 'NONE', ( #18333 ), #4956, .F. ) ;
#3889 = CARTESIAN_POINT ( 'NONE',  ( -35.00000000000001421, 84.70000000000001705, 78.79999999999999716 ) ) ;
#3890 = AXIS2_PLACEMENT_3D ( 'NONE', #8812, #5244, #12149 ) ;
#3891 = AXIS2_PLACEMENT_3D ( 'NONE', #2960, #15137, #21983 ) ;
#3892 = CARTESIAN_POINT ( 'NONE',  ( -18.22752199202934520, -38.74634676501045760, 13.50000000000000000 ) ) ;
#3893 = VECTOR ( 'NONE', #7183, 1000.000000000000000 ) ;
#3894 = DIRECTION ( 'NONE',  ( -1.000000000000000000, 0.000000000000000000, -0.000000000000000000 ) ) ;
#3895 = ORIENTED_EDGE ( 'NONE', *, *, #10755, .F. ) ;
#3896 = DIRECTION ( 'NONE',  ( -1.000000000000000000, -0.000000000000000000, -0.000000000000000000 ) ) ;
#3897 = AXIS2_PLACEMENT_3D ( 'NONE', #8496, #15315, #13632 ) ;
#3898 = CARTESIAN_POINT ( 'NONE',  ( -32.50000000000002132, 72.00000000000001421, 3.500000000000000000 ) ) ;
#3899 = CARTESIAN_POINT ( 'NONE',  ( -9.178906393579158163, 42.46645089659918426, 70.88527860057354246 ) ) ;
#3900 = DIRECTION ( 'NONE',  ( 0.000000000000000000, 0.000000000000000000, -1.000000000000000000 ) ) ;
#3901 = ORIENTED_EDGE ( 'NONE', *, *, #14416, .F. ) ;
#3902 = CARTESIAN_POINT ( 'NONE',  ( -8.149501154770145916, 43.00645089659919051, 70.88527860057354246 ) ) ;
#3903 = ORIENTED_EDGE ( 'NONE', *, *, #2311, .F. ) ;
#3904 = LINE ( 'NONE', #9140, #4117 ) ;
#3905 = DIRECTION ( 'NONE',  ( -1.000000000000000000, -0.000000000000000000, -0.000000000000000000 ) ) ;
#3906 = AXIS2_PLACEMENT_3D ( 'NONE', #5246, #3773, #1876 ) ;
#3907 = ORIENTED_EDGE ( 'NONE', *, *, #10331, .F. ) ;
#3908 = EDGE_LOOP ( 'NONE', ( #9178, #10832, #16671, #20587 ) ) ;
#3909 = EDGE_CURVE ( 'NONE', #6564, #8381, #10674, .T. ) ;
#3910 = DIRECTION ( 'NONE',  ( 0.000000000000000000, 0.000000000000000000, 1.000000000000000000 ) ) ;
#3911 = VECTOR ( 'NONE', #20198, 1000.000000000000000 ) ;
#3912 = ORIENTED_EDGE ( 'NONE', *, *, #3231, .F. ) ;
#3913 = AXIS2_PLACEMENT_3D ( 'NONE', #14493, #21474, #19668 ) ;
#3914 = EDGE_LOOP ( 'NONE', ( #2224, #427, #9989, #605 ) ) ;
#3915 = EDGE_CURVE ( 'NONE', #823, #17660, #11942, .T. ) ;
#3916 = EDGE_CURVE ( 'NONE', #12157, #12641, #8379, .T. ) ;
#3917 = EDGE_LOOP ( 'NONE', ( #14464, #11582, #17423, #22009, #17487, #19583, #272, #13952 ) ) ;
#3918 = DIRECTION ( 'NONE',  ( 0.000000000000000000, 0.000000000000000000, 1.000000000000000000 ) ) ;
#3919 = ADVANCED_FACE ( 'NONE', ( #10065 ), #22042, .F. ) ;
#3920 = DIRECTION ( 'NONE',  ( 1.000000000000000000, 0.000000000000000000, 0.000000000000000000 ) ) ;
#3921 = CARTESIAN_POINT ( 'NONE',  ( 28.90801073195815718, 6.496214187273303686, 7.643093741255248652 ) ) ;
#3922 = EDGE_CURVE ( 'NONE', #12867, #12488, #5032, .T. ) ;
#3923 = FACE_OUTER_BOUND ( 'NONE', #10614, .T. ) ;
#3924 = AXIS2_PLACEMENT_3D ( 'NONE', #11851, #10184, #6852 ) ;
#3925 = DIRECTION ( 'NONE',  ( 0.000000000000000000, 0.000000000000000000, -1.000000000000000000 ) ) ;
#3926 = ORIENTED_EDGE ( 'NONE', *, *, #16346, .T. ) ;
#3927 = CARTESIAN_POINT ( 'NONE',  ( -32.20000000000001705, 0.000000000000000000, 1.800000000000000044 ) ) ;
#3928 = CYLINDRICAL_SURFACE ( 'NONE', #19808, 0.09999999999999939493 ) ;
#3929 = DIRECTION ( 'NONE',  ( -0.000000000000000000, 0.000000000000000000, 1.000000000000000000 ) ) ;
#3930 = ORIENTED_EDGE ( 'NONE', *, *, #11414, .T. ) ;
#3931 = ADVANCED_FACE ( 'NONE', ( #11832 ), #1653, .F. ) ;
#3932 = LINE ( 'NONE', #7619, #4564 ) ;
#3933 = ORIENTED_EDGE ( 'NONE', *, *, #13752, .T. ) ;
#3934 = ORIENTED_EDGE ( 'NONE', *, *, #11504, .F. ) ;
#3935 = DIRECTION ( 'NONE',  ( 0.000000000000000000, 1.000000000000000000, 0.000000000000000000 ) ) ;
#3936 = CONTEXT_DEPENDENT_SHAPE_REPRESENTATION ( #17286, #1802 ) ;
#3937 = ORIENTED_EDGE ( 'NONE', *, *, #14119, .F. ) ;
#3938 = AXIS2_PLACEMENT_3D ( 'NONE', #21110, #7019, #387 ) ;
#3939 = ORIENTED_EDGE ( 'NONE', *, *, #7876, .F. ) ;
#3940 = CARTESIAN_POINT ( 'NONE',  ( 23.04273161205366449, -2.261511134070602225, 13.23413512703649531 ) ) ;
#3941 = ORIENTED_EDGE ( 'NONE', *, *, #21945, .T. ) ;
#3942 = EDGE_CURVE ( 'NONE', #17693, #2296, #19254, .T. ) ;
#3943 = VERTEX_POINT ( 'NONE', #5712 ) ;
#3944 = ADVANCED_FACE ( 'NONE', ( #12374 ), #3184, .T. ) ;
#3945 = CARTESIAN_POINT ( 'NONE',  ( -32.50000000000002132, -71.00000000000001421, 3.500000000000000000 ) ) ;
#3946 = DIRECTION ( 'NONE',  ( 0.000000000000000000, -1.000000000000000000, 0.000000000000000000 ) ) ;
#3947 = FACE_OUTER_BOUND ( 'NONE', #1316, .T. ) ;
#3948 = DIRECTION ( 'NONE',  ( 0.000000000000000000, -1.000000000000000000, 0.000000000000000000 ) ) ;
#3949 = CARTESIAN_POINT ( 'NONE',  ( -32.20000000000001705, -71.00000000000001421, 3.200000000000000178 ) ) ;
#3950 = CIRCLE ( 'NONE', #19308, 1.000000000000000888 ) ;
#3951 = COLOUR_RGB ( '', 0.08235294, 0.09019608, 0.10196078) ;
#3952 = DIRECTION ( 'NONE',  ( -1.000000000000000000, 0.000000000000000000, 0.000000000000000000 ) ) ;
#3953 = PLANE ( 'NONE',  #9019 ) ;
#3954 = CARTESIAN_POINT ( 'NONE',  ( 23.14079623692856202, -2.756488901337828423, 13.42422799743261130 ) ) ;
#3955 = CARTESIAN_POINT ( 'NONE',  ( -25.37540678000426908, 36.74634676501047181, 13.79999999999999893 ) ) ;
#3956 = CARTESIAN_POINT ( 'NONE',  ( 30.37540678000427619, -63.74634676501045050, 7.200000000000000178 ) ) ;
#3957 = ORIENTED_EDGE ( 'NONE', *, *, #13340, .F. ) ;
#3958 = ORIENTED_EDGE ( 'NONE', *, *, #21151, .F. ) ;
#3959 = DIRECTION ( 'NONE',  ( 1.000000000000000000, 0.000000000000000000, 0.000000000000000000 ) ) ;
#3960 =( LENGTH_UNIT ( ) NAMED_UNIT ( * ) SI_UNIT ( .MILLI., .METRE. ) );
#3962 = EDGE_CURVE ( 'NONE', #1897, #17480, #17113, .T. ) ;
#3961 = DIRECTION ( 'NONE',  ( 1.000000000000000000, 0.000000000000000000, 0.000000000000000000 ) ) ;
#3963 = ADVANCED_FACE ( 'NONE', ( #2100 ), #5483, .F. ) ;
#3964 = ORIENTED_EDGE ( 'NONE', *, *, #4895, .F. ) ;
#3965 = VERTEX_POINT ( 'NONE', #1978 ) ;
#3966 = VECTOR ( 'NONE', #15376, 1000.000000000000000 ) ;
#3967 = VECTOR ( 'NONE', #4270, 1000.000000000000000 ) ;
#3968 = ADVANCED_FACE ( 'NONE', ( #7368 ), #19981, .T. ) ;
#3969 = DIRECTION ( 'NONE',  ( 0.000000000000000000, 0.000000000000000000, -1.000000000000000000 ) ) ;
#3970 = CARTESIAN_POINT ( 'NONE',  ( 31.69597781366222122, 56.94165929845684104, 70.50000000000000000 ) ) ;
#3971 = ORIENTED_EDGE ( 'NONE', *, *, #15440, .F. ) ;
#3972 = DIRECTION ( 'NONE',  ( 0.000000000000000000, -1.000000000000000000, 0.000000000000000000 ) ) ;
#3973 = CARTESIAN_POINT ( 'NONE',  ( 14.96174975910705918, 41.81054587065082728, 13.80000000000001315 ) ) ;
#3974 = CARTESIAN_POINT ( 'NONE',  ( -32.23382792203229741, 83.71979900898287497, 13.75000000000000000 ) ) ;
#3975 = CARTESIAN_POINT ( 'NONE',  ( 9.641460742840918030, -32.11873716947361856, 42.50000000000000711 ) ) ;
#3976 = CYLINDRICAL_SURFACE ( 'NONE', #21521, 0.3000000000000001554 ) ;
#3977 = DIRECTION ( 'NONE',  ( 0.000000000000000000, -0.000000000000000000, -1.000000000000000000 ) ) ;
#3978 = LINE ( 'NONE', #19628, #19350 ) ;
#3979 = VECTOR ( 'NONE', #20492, 1000.000000000000000 ) ;
#3980 = CARTESIAN_POINT ( 'NONE',  ( -17.45292532278785913, 50.11873716947361856, 68.50000000000000000 ) ) ;
#3981 = DIRECTION ( 'NONE',  ( 0.000000000000000000, -1.000000000000000000, 0.000000000000000000 ) ) ;
#3982 = ORIENTED_EDGE ( 'NONE', *, *, #9955, .T. ) ;
#3983 = VERTEX_POINT ( 'NONE', #14289 ) ;
#3984 = VERTEX_POINT ( 'NONE', #19337 ) ;
#3985 = CARTESIAN_POINT ( 'NONE',  ( -28.87540678000427619, -6.494748934539263274, 7.720760502796167657 ) ) ;
#3987 = ADVANCED_FACE ( 'NONE', ( #17543 ), #17642, .F. ) ;
#3986 = DIRECTION ( 'NONE',  ( -1.000000000000000000, 0.000000000000000000, 0.000000000000000000 ) ) ;
#3988 = ORIENTED_EDGE ( 'NONE', *, *, #21149, .T. ) ;
#3989 = EDGE_CURVE ( 'NONE', #19805, #2320, #660, .T. ) ;
#3990 = PLANE ( 'NONE',  #17070 ) ;
#3991 = VECTOR ( 'NONE', #5102, 1000.000000000000000 ) ;
#3992 = AXIS2_PLACEMENT_3D ( 'NONE', #11218, #6104, #16579 ) ;
#3993 = ORIENTED_EDGE ( 'NONE', *, *, #1861, .F. ) ;
#3994 = CARTESIAN_POINT ( 'NONE',  ( 0.000000000000000000, 43.26054587065083012, 37.71679706732590631 ) ) ;
#3995 = SHAPE_REPRESENTATION ( 'Light', ( #17493 ), #14991 ) ;
#3996 = DIRECTION ( 'NONE',  ( 0.000000000000000000, 0.000000000000000000, 1.000000000000000000 ) ) ;
#3997 = ORIENTED_EDGE ( 'NONE', *, *, #8473, .F. ) ;
#3998 = CARTESIAN_POINT ( 'NONE',  ( -23.04273156199908357, -2.261510999192740901, 13.19999999999999929 ) ) ;
#3999 = FACE_OUTER_BOUND ( 'NONE', #750, .T. ) ;
#4000 = CARTESIAN_POINT ( 'NONE',  ( -24.94594744299175915, 42.46645089659918426, 13.74999999999999822 ) ) ;
#4001 = DIRECTION ( 'NONE',  ( 0.000000000000000000, -1.000000000000000000, 0.000000000000000000 ) ) ;
#4002 = ORIENTED_EDGE ( 'NONE', *, *, #10244, .F. ) ;
#4003 = CYLINDRICAL_SURFACE ( 'NONE', #15922, 0.1000000000000028644 ) ;
#4004 = DIRECTION ( 'NONE',  ( 1.000000000000000000, 0.000000000000000000, 0.000000000000000000 ) ) ;
#4005 = DIRECTION ( 'NONE',  ( 0.000000000000000000, 1.000000000000000000, -0.000000000000000000 ) ) ;
#4006 = CARTESIAN_POINT ( 'NONE',  ( 14.96174975910707161, 51.61873716947361856, 68.25000000000000000 ) ) ;
#4007 = VERTEX_POINT ( 'NONE', #15518 ) ;
#4008 = EDGE_CURVE ( 'NONE', #11811, #11228, #187, .T. ) ;
#4009 =( NAMED_UNIT ( * ) SI_UNIT ( $, .STERADIAN. ) SOLID_ANGLE_UNIT ( ) );
#4010 = AXIS2_PLACEMENT_3D ( 'NONE', #14024, #17381, #14249 ) ;
#4011 = ORIENTED_EDGE ( 'NONE', *, *, #2853, .T. ) ;
#4012 = DIRECTION ( 'NONE',  ( 0.000000000000000000, 0.000000000000000000, 1.000000000000000000 ) ) ;
#4013 = CARTESIAN_POINT ( 'NONE',  ( 3.127054932750481964, 32.93424481021354921, 68.50000000000000000 ) ) ;
#4014 = ORIENTED_EDGE ( 'NONE', *, *, #5879, .T. ) ;
#4015 = ORIENTED_EDGE ( 'NONE', *, *, #4115, .T. ) ;
#4016 = DIRECTION ( 'NONE',  ( -1.000000000000000000, 0.000000000000000000, 0.000000000000000000 ) ) ;
#4017 = EDGE_CURVE ( 'NONE', #16466, #7129, #10610, .T. ) ;
#4018 = EDGE_CURVE ( 'NONE', #15927, #1798, #13881, .T. ) ;
#4019 = DIRECTION ( 'NONE',  ( -0.000000000000000000, -0.000000000000000000, -1.000000000000000000 ) ) ;
#4020 = ORIENTED_EDGE ( 'NONE', *, *, #1216, .F. ) ;
#4021 = EDGE_LOOP ( 'NONE', ( #15747, #14061, #12694, #2654 ) ) ;
#4022 = AXIS2_PLACEMENT_3D ( 'NONE', #560, #8873, #15786 ) ;
#4023 = CARTESIAN_POINT ( 'NONE',  ( 1.774728116533979883, 42.36054587065083155, 33.66679706732590915 ) ) ;
#4024 = CYLINDRICAL_SURFACE ( 'NONE', #1335, 0.2500000000000002220 ) ;
#4025 = VECTOR ( 'NONE', #20915, 1000.000000000000227 ) ;
#4026 = FACE_OUTER_BOUND ( 'NONE', #19577, .T. ) ;
#4027 = DIRECTION ( 'NONE',  ( 1.000000000000000000, -0.000000000000000000, -0.000000000000000000 ) ) ;
#4028 = DIRECTION ( 'NONE',  ( 0.000000000000000000, 0.000000000000000000, 1.000000000000000000 ) ) ;
#4029 = ADVANCED_FACE ( 'NONE', ( #15952 ), #5372, .T. ) ;
#4030 = EDGE_LOOP ( 'NONE', ( #15499, #14800, #11070, #20164 ) ) ;
#4031 = DIRECTION ( 'NONE',  ( -0.000000000000000000, -0.000000000000000000, 1.000000000000000000 ) ) ;
#4032 = FACE_OUTER_BOUND ( 'NONE', #5420, .T. ) ;
#4033 = LINE ( 'NONE', #7177, #21551 ) ;
#4034 = ORIENTED_EDGE ( 'NONE', *, *, #16966, .F. ) ;
#4035 = EDGE_CURVE ( 'NONE', #17520, #897, #11384, .T. ) ;
#4036 = ORIENTED_EDGE ( 'NONE', *, *, #1885, .T. ) ;
#4037 = ADVANCED_FACE ( 'NONE', ( #850 ), #4607, .T. ) ;
#4038 = VERTEX_POINT ( 'NONE', #4440 ) ;
#4039 = ORIENTED_EDGE ( 'NONE', *, *, #2990, .T. ) ;
#4040 = FACE_OUTER_BOUND ( 'NONE', #11642, .T. ) ;
#4041 = ORIENTED_EDGE ( 'NONE', *, *, #14572, .T. ) ;
#4042 = VERTEX_POINT ( 'NONE', #6251 ) ;
#4043 = LINE ( 'NONE', #9070, #7588 ) ;
#4044 = ORIENTED_EDGE ( 'NONE', *, *, #16723, .T. ) ;
#4045 = DIRECTION ( 'NONE',  ( 0.000000000000000000, 0.000000000000000000, -1.000000000000000000 ) ) ;
#4046 = FACE_OUTER_BOUND ( 'NONE', #3032, .T. ) ;
#4047 = DIRECTION ( 'NONE',  ( 0.000000000000000000, 1.000000000000000000, 0.000000000000000000 ) ) ;
#4048 = EDGE_CURVE ( 'NONE', #6536, #8703, #10689, .T. ) ;
#4049 = DIRECTION ( 'NONE',  ( 1.000000000000000000, 0.000000000000000000, 0.000000000000000000 ) ) ;
#4050 = CARTESIAN_POINT ( 'NONE',  ( 34.39999999999998437, 84.70000000000001705, 79.39999999999999147 ) ) ;
#4051 = FACE_OUTER_BOUND ( 'NONE', #14789, .T. ) ;
#4052 = CYLINDRICAL_SURFACE ( 'NONE', #19019, 0.5000000000000004441 ) ;
#4053 = CARTESIAN_POINT ( 'NONE',  ( -25.37540678000426908, 39.04634676501046187, 13.79999999999999893 ) ) ;
#4054 = CARTESIAN_POINT ( 'NONE',  ( 15.21174975910705918, 42.31054587065082728, 13.75000000000000000 ) ) ;
#4055 = EDGE_CURVE ( 'NONE', #16591, #13276, #7844, .T. ) ;
#4056 = ADVANCED_FACE ( 'NONE', ( #14390 ), #4228, .T. ) ;
#4057 =( GEOMETRIC_REPRESENTATION_CONTEXT ( 3 ) GLOBAL_UNCERTAINTY_ASSIGNED_CONTEXT ( ( #1994 ) ) GLOBAL_UNIT_ASSIGNED_CONTEXT ( ( #571, #12757, #14230 ) ) REPRESENTATION_CONTEXT ( 'NONE', 'WORKASPACE' ) );
#4058 = VERTEX_POINT ( 'NONE', #7692 ) ;
#4059 = VERTEX_POINT ( 'NONE', #6032 ) ;
#4060 = CARTESIAN_POINT ( 'NONE',  ( -11.62890639357915923, 43.00645089659917630, 70.88527860057354246 ) ) ;
#4061 = EDGE_CURVE ( 'NONE', #21319, #10096, #16411, .T. ) ;
#4062 = ORIENTED_EDGE ( 'NONE', *, *, #18303, .T. ) ;
#4063 = VERTEX_POINT ( 'NONE', #4337 ) ;
#4064 = ORIENTED_EDGE ( 'NONE', *, *, #21581, .F. ) ;
#4065 = DIRECTION ( 'NONE',  ( -1.000000000000000000, 0.000000000000000000, -0.000000000000000000 ) ) ;
#4066 = LINE ( 'NONE', #10883, #11993 ) ;
#4067 = ORIENTED_EDGE ( 'NONE', *, *, #19613, .T. ) ;
#4068 = LINE ( 'NONE', #699, #717 ) ;
#4069 = CARTESIAN_POINT ( 'NONE',  ( -23.32398829872514057, 2.157133568460765982, 13.19999999999999929 ) ) ;
#4070 = EDGE_CURVE ( 'NONE', #18637, #16490, #19779, .T. ) ;
#4071 = DIRECTION ( 'NONE',  ( 0.000000000000000000, 0.000000000000000000, 1.000000000000000000 ) ) ;
#4072 = CARTESIAN_POINT ( 'NONE',  ( 15.12813070831323969, 51.99253567353609640, 13.49999999999999822 ) ) ;
#4073 = DIRECTION ( 'NONE',  ( 1.000000000000000000, -0.000000000000000000, -0.000000000000000000 ) ) ;
#4074 = CARTESIAN_POINT ( 'NONE',  ( -25.37540678000427263, -69.04634676501045476, 3.500000000000000000 ) ) ;
#4075 = AXIS2_PLACEMENT_3D ( 'NONE', #4100, #948, #9358 ) ;
#4076 = CARTESIAN_POINT ( 'NONE',  ( -1.724728116533986721, 43.31054587065082728, 35.80876104995653009 ) ) ;
#4077 = DIRECTION ( 'NONE',  ( -1.000000000000000000, 0.000000000000000000, -0.000000000000000000 ) ) ;
#4078 = LINE ( 'NONE', #7559, #18845 ) ;
#4079 = ORIENTED_EDGE ( 'NONE', *, *, #6560, .F. ) ;
#4080 = EDGE_LOOP ( 'NONE', ( #8945, #7643, #6808, #17593 ) ) ;
#4081 = EDGE_LOOP ( 'NONE', ( #11201, #10599, #2640, #14360 ) ) ;
#4082 = LINE ( 'NONE', #2068, #240 ) ;
#4083 = EDGE_CURVE ( 'NONE', #8790, #18066, #21418, .T. ) ;
#4084 = PLANE ( 'NONE',  #22127 ) ;
#4085 = VERTEX_POINT ( 'NONE', #14730 ) ;
#4086 = VECTOR ( 'NONE', #5454, 1000.000000000000000 ) ;
#4087 = CYLINDRICAL_SURFACE ( 'NONE', #14197, 2.500000000000000444 ) ;
#4088 = AXIS2_PLACEMENT_3D ( 'NONE', #15808, #19298, #9105 ) ;
#4089 = VERTEX_POINT ( 'NONE', #2887 ) ;
#4090 = CARTESIAN_POINT ( 'NONE',  ( -1.824728116533986810, 43.31054587065082728, 33.66679706732590915 ) ) ;
#4091 = DIRECTION ( 'NONE',  ( 1.000000000000000000, 0.000000000000000000, 0.000000000000000000 ) ) ;
#4092 = CARTESIAN_POINT ( 'NONE',  ( -28.71290943744531177, -6.649236572130504896, 13.47739020623642325 ) ) ;
#4093 = DIRECTION ( 'NONE',  ( 1.000000000000000000, 0.000000000000000000, 0.000000000000000000 ) ) ;
#4094 = CARTESIAN_POINT ( 'NONE',  ( -1.724728116533986721, 43.31054587065082728, 31.75876104995653648 ) ) ;
#4095 = FACE_OUTER_BOUND ( 'NONE', #6845, .T. ) ;
#4096 = ORIENTED_EDGE ( 'NONE', *, *, #19214, .F. ) ;
#4097 = LINE ( 'NONE', #6016, #18073 ) ;
#4098 = DIRECTION ( 'NONE',  ( 1.000000000000000000, 0.000000000000000000, 0.000000000000000000 ) ) ;
#4099 = EDGE_CURVE ( 'NONE', #8904, #7257, #14603, .T. ) ;
#4100 = CARTESIAN_POINT ( 'NONE',  ( -27.37540678000427619, 7.754037881813018962E-15, 42.50000000000000000 ) ) ;
#4101 = CARTESIAN_POINT ( 'NONE',  ( -1.824728116533986810, 43.31054587065082728, 43.70876104995653577 ) ) ;
#4102 = VERTEX_POINT ( 'NONE', #7928 ) ;
#4103 = EDGE_CURVE ( 'NONE', #8181, #4433, #9372, .T. ) ;
#4104 = DIRECTION ( 'NONE',  ( 1.000000000000000000, 0.000000000000000000, 0.000000000000000000 ) ) ;
#4105 = VECTOR ( 'NONE', #5415, 1000.000000000000114 ) ;
#4106 = ORIENTED_EDGE ( 'NONE', *, *, #18160, .T. ) ;
#4107 = DIRECTION ( 'NONE',  ( -0.000000000000000000, -0.000000000000000000, -1.000000000000000000 ) ) ;
#4108 = DIRECTION ( 'NONE',  ( 1.000000000000000000, 0.000000000000000000, 0.000000000000000000 ) ) ;
#4109 = ORIENTED_EDGE ( 'NONE', *, *, #983, .F. ) ;
#4110 = EDGE_LOOP ( 'NONE', ( #3323, #15325, #9629, #15369 ) ) ;
#4111 = CARTESIAN_POINT ( 'NONE',  ( -14.71174975910705029, 0.000000000000000000, 68.25000000000000000 ) ) ;
#4112 = CARTESIAN_POINT ( 'NONE',  ( -0.000000000000000000, 51.61873716947361856, 68.50000000000000000 ) ) ;
#4113 = VERTEX_POINT ( 'NONE', #11375 ) ;
#4114 = ORIENTED_EDGE ( 'NONE', *, *, #21927, .F. ) ;
#4115 = EDGE_CURVE ( 'NONE', #8087, #538, #6730, .T. ) ;
#4116 = EDGE_CURVE ( 'NONE', #16814, #2496, #744, .T. ) ;
#4117 = VECTOR ( 'NONE', #10606, 1000.000000000000000 ) ;
#4118 = AXIS2_PLACEMENT_3D ( 'NONE', #10061, #21820, #6605 ) ;
#4119 = VERTEX_POINT ( 'NONE', #16068 ) ;
#4120 = DIRECTION ( 'NONE',  ( 0.2309407893632139108, -0.9729678061520308230, 0.000000000000000000 ) ) ;
#4121 = LINE ( 'NONE', #2221, #7958 ) ;
#4122 = FACE_OUTER_BOUND ( 'NONE', #8279, .T. ) ;
#4123 = ADVANCED_FACE ( 'NONE', ( #1181 ), #18487, .T. ) ;
#4124 = DIRECTION ( 'NONE',  ( -1.000000000000000000, 0.000000000000000000, 0.000000000000000000 ) ) ;
#4125 = CARTESIAN_POINT ( 'NONE',  ( -9.141460742840918030, -32.61873716947361856, 68.00000000000000000 ) ) ;
#4126 = VERTEX_POINT ( 'NONE', #7820 ) ;
#4127 = AXIS2_PLACEMENT_3D ( 'NONE', #7840, #12837, #16433 ) ;
#4128 = FACE_OUTER_BOUND ( 'NONE', #5758, .T. ) ;
#4129 = PLANE ( 'NONE',  #19747 ) ;
#4130 = CIRCLE ( 'NONE', #16621, 0.04999999999999991257 ) ;
#4131 = AXIS2_PLACEMENT_3D ( 'NONE', #10794, #8686, #17609 ) ;
#4132 = TOROIDAL_SURFACE ( 'NONE', #10567, 5.193574995607837863, 1.000000000000000000 ) ;
#4133 = ORIENTED_EDGE ( 'NONE', *, *, #20262, .T. ) ;
#4134 = DIRECTION ( 'NONE',  ( 0.000000000000000000, 0.000000000000000000, 1.000000000000000000 ) ) ;
#4135 = ORIENTED_EDGE ( 'NONE', *, *, #16489, .F. ) ;
#4136 = ORIENTED_EDGE ( 'NONE', *, *, #4103, .T. ) ;
#4137 = CARTESIAN_POINT ( 'NONE',  ( 14.71174975910705740, 51.61873716947361856, 13.50000000000000000 ) ) ;
#4138 = ITEM_DEFINED_TRANSFORMATION ( 'NONE', 'NONE', #6586,  #17493 ) ;
#4139 = ADVANCED_FACE ( 'NONE', ( #12596 ), #19439, .T. ) ;
#4140 = ORIENTED_EDGE ( 'NONE', *, *, #6373, .F. ) ;
#4141 = VERTEX_POINT ( 'NONE', #2543 ) ;
#4142 = VECTOR ( 'NONE', #4857, 1000.000000000000000 ) ;
#4143 = CYLINDRICAL_SURFACE ( 'NONE', #9365, 0.2500000000000002220 ) ;
#4144 = ORIENTED_EDGE ( 'NONE', *, *, #18101, .F. ) ;
#4145 = CARTESIAN_POINT ( 'NONE',  ( -25.37540678000427263, -68.74634676501045760, 3.799999999999999822 ) ) ;
#4146 = CIRCLE ( 'NONE', #10586, 0.05000000000000143219 ) ;
#4147 = ORIENTED_EDGE ( 'NONE', *, *, #8333, .F. ) ;
#4148 = EDGE_CURVE ( 'NONE', #627, #12433, #6479, .T. ) ;
#4149 = CARTESIAN_POINT ( 'NONE',  ( 30.67540678000428045, -63.74634676501045050, 3.799999999999999822 ) ) ;
#4150 = FACE_OUTER_BOUND ( 'NONE', #15721, .T. ) ;
#4151 = CARTESIAN_POINT ( 'NONE',  ( -4.127054932750482408, 33.93424481021354921, 68.50000000000000000 ) ) ;
#4152 = ADVANCED_FACE ( 'NONE', ( #8467 ), #22139, .T. ) ;
#4153 = DIRECTION ( 'NONE',  ( -0.000000000000000000, 0.000000000000000000, -1.000000000000000000 ) ) ;
#4154 = DIRECTION ( 'NONE',  ( -1.000000000000000000, 0.000000000000000000, 0.000000000000000000 ) ) ;
#4155 = DIRECTION ( 'NONE',  ( 1.000000000000000000, 2.832483164223434527E-16, -0.000000000000000000 ) ) ;
#4156 = CARTESIAN_POINT ( 'NONE',  ( -1.724728116533986721, 42.36054587065083155, 27.80876104995653719 ) ) ;
#4157 = LINE ( 'NONE', #14333, #7544 ) ;
#4158 = CIRCLE ( 'NONE', #1988, 0.1000000000000028644 ) ;
#4159 = CIRCLE ( 'NONE', #14161, 0.2999999999999999334 ) ;
#4160 = TOROIDAL_SURFACE ( 'NONE', #20249, 5.300000000000004263, 0.2999999999999999889 ) ;
#4161 = DIRECTION ( 'NONE',  ( -0.000000000000000000, 0.000000000000000000, 1.000000000000000000 ) ) ;
#4162 = ORIENTED_EDGE ( 'NONE', *, *, #8286, .T. ) ;
#4163 = AXIS2_PLACEMENT_3D ( 'NONE', #17815, #9529, #21628 ) ;
#4164 = ORIENTED_EDGE ( 'NONE', *, *, #16909, .F. ) ;
#4165 = LINE ( 'NONE', #21193, #10313 ) ;
#4166 = PLANE ( 'NONE',  #7070 ) ;
#4167 = EDGE_CURVE ( 'NONE', #15663, #7855, #1703, .T. ) ;
#4168 = ORIENTED_EDGE ( 'NONE', *, *, #4594, .F. ) ;
#4169 = EDGE_LOOP ( 'NONE', ( #20693, #9227, #5059, #16687 ) ) ;
#4170 = VECTOR ( 'NONE', #18291, 1000.000000000000000 ) ;
#4171 = VECTOR ( 'NONE', #17267, 1000.000000000000000 ) ;
#4172 = TOROIDAL_SURFACE ( 'NONE', #18110, 0.7000000000000000666, 0.2999999999999999889 ) ;
#4173 = CARTESIAN_POINT ( 'NONE',  ( -14.71432562863492066, -52.07267296161941061, 13.50000000000000000 ) ) ;
#4174 = EDGE_CURVE ( 'NONE', #14884, #19733, #2778, .T. ) ;
#4175 = DIRECTION ( 'NONE',  ( -0.000000000000000000, 1.000000000000000000, -0.000000000000000000 ) ) ;
#4176 = CIRCLE ( 'NONE', #2031, 0.2999999999999999334 ) ;
#4177 = ORIENTED_EDGE ( 'NONE', *, *, #12589, .F. ) ;
#4178 = CARTESIAN_POINT ( 'NONE',  ( 17.93704824106378837, -50.11873716947361856, 13.87500000000000000 ) ) ;
#4179 = ADVANCED_FACE ( 'NONE', ( #16739 ), #797, .F. ) ;
#4180 = DIRECTION ( 'NONE',  ( 1.000000000000000000, 0.000000000000000000, 0.000000000000000000 ) ) ;
#4181 = DIRECTION ( 'NONE',  ( -0.000000000000000000, -1.000000000000000000, -0.000000000000000000 ) ) ;
#4182 = CARTESIAN_POINT ( 'NONE',  ( 1.824728116533979705, 43.26054587065083012, 37.66679706732590915 ) ) ;
#4183 = CARTESIAN_POINT ( 'NONE',  ( -23.11756190325308680, 2.646657027129579287, 13.40142076604336019 ) ) ;
#4184 = EDGE_LOOP ( 'NONE', ( #10489, #7725, #9473, #18017, #18498, #2549, #3339, #741 ) ) ;
#4185 = DIRECTION ( 'NONE',  ( 0.000000000000000000, -0.000000000000000000, 1.000000000000000000 ) ) ;
#4186 = CARTESIAN_POINT ( 'NONE',  ( -21.92816239687475743, 42.46645089659918426, 68.25000000000000000 ) ) ;
#4187 = AXIS2_PLACEMENT_3D ( 'NONE', #8975, #19271, #3828 ) ;
#4188 = CYLINDRICAL_SURFACE ( 'NONE', #9541, 0.2999999999999999334 ) ;
#4189 = ORIENTED_EDGE ( 'NONE', *, *, #7989, .F. ) ;
#4190 = VECTOR ( 'NONE', #11614, 1000.000000000000000 ) ;
#4191 = AXIS2_PLACEMENT_3D ( 'NONE', #14310, #7390, #4134 ) ;
#4192 = ORIENTED_EDGE ( 'NONE', *, *, #14300, .T. ) ;
#4193 = EDGE_LOOP ( 'NONE', ( #20995, #12184, #15162, #16561 ) ) ;
#4194 = CARTESIAN_POINT ( 'NONE',  ( -29.20000000000002061, 0.000000000000000000, 0.2999999999999947153 ) ) ;
#4195 = DIRECTION ( 'NONE',  ( 0.000000000000000000, 0.000000000000000000, -1.000000000000000000 ) ) ;
#4196 = EDGE_CURVE ( 'NONE', #21191, #21353, #16337, .T. ) ;
#4197 = CIRCLE ( 'NONE', #4921, 1.000000000000000000 ) ;
#4198 = DIRECTION ( 'NONE',  ( -1.000000000000000000, 0.000000000000000000, -0.000000000000000000 ) ) ;
#4199 = AXIS2_PLACEMENT_3D ( 'NONE', #5318, #10451, #20522 ) ;
#4200 = ORIENTED_EDGE ( 'NONE', *, *, #13550, .F. ) ;
#4201 = CARTESIAN_POINT ( 'NONE',  ( 9.641460742840918030, 32.61873716947361856, 109.6002446535588319 ) ) ;
#4202 = CARTESIAN_POINT ( 'NONE',  ( -11.67890639357916172, 42.46645089659918426, 61.53912392244307483 ) ) ;
#4203 = CARTESIAN_POINT ( 'NONE',  ( -14.71174975910705029, 50.19799549595485644, 13.50000000000000000 ) ) ;
#4204 = LINE ( 'NONE', #21333, #4939 ) ;
#4205 = ADVANCED_FACE ( 'NONE', ( #5965 ), #20554, .F. ) ;
#4206 = AXIS2_PLACEMENT_3D ( 'NONE', #16886, #3464, #3133 ) ;
#4207 = AXIS2_PLACEMENT_3D ( 'NONE', #8946, #10834, #2325 ) ;
#4208 = AXIS2_PLACEMENT_3D ( 'NONE', #18334, #9499, #4464 ) ;
#4209 = PLANE ( 'NONE',  #15060 ) ;
#4210 = CARTESIAN_POINT ( 'NONE',  ( -1.774728116533986766, 43.26054587065083012, 8.000000000000000000 ) ) ;
#4211 = ORIENTED_EDGE ( 'NONE', *, *, #21024, .T. ) ;
#4212 = DIRECTION ( 'NONE',  ( -1.000000000000000000, 0.000000000000000000, 0.000000000000000000 ) ) ;
#4213 = EDGE_CURVE ( 'NONE', #14801, #5317, #10996, .T. ) ;
#4214 = DIRECTION ( 'NONE',  ( -0.000000000000000000, -1.000000000000000000, -0.000000000000000000 ) ) ;
#4215 = VECTOR ( 'NONE', #17123, 1000.000000000000000 ) ;
#4216 = CARTESIAN_POINT ( 'NONE',  ( -29.69597781366221412, 25.99124249474150972, 70.25000000000000000 ) ) ;
#4217 = CARTESIAN_POINT ( 'NONE',  ( -23.11743451022279316, -2.646042693280195923, 13.40127653599240887 ) ) ;
#4218 = ORIENTED_EDGE ( 'NONE', *, *, #10183, .T. ) ;
#4219 =( LENGTH_UNIT ( ) NAMED_UNIT ( * ) SI_UNIT ( .MILLI., .METRE. ) );
#4220 = AXIS2_PLACEMENT_3D ( 'NONE', #18257, #21528, #16461 ) ;
#4221 = DIRECTION ( 'NONE',  ( -1.000000000000000000, 0.000000000000000000, 0.000000000000000000 ) ) ;
#4222 = AXIS2_PLACEMENT_3D ( 'NONE', #9420, #19950, #21525 ) ;
#4223 = EDGE_LOOP ( 'NONE', ( #16220, #5972, #20805, #1103 ) ) ;
#4224 = CYLINDRICAL_SURFACE ( 'NONE', #6992, 0.2999999999999999889 ) ;
#4225 = DIRECTION ( 'NONE',  ( 0.000000000000000000, -1.000000000000000000, -0.000000000000000000 ) ) ;
#4226 = ORIENTED_EDGE ( 'NONE', *, *, #17322, .T. ) ;
#4227 = ORIENTED_EDGE ( 'NONE', *, *, #12070, .F. ) ;
#4228 = CYLINDRICAL_SURFACE ( 'NONE', #20344, 0.1000000000000028644 ) ;
#4229 = CARTESIAN_POINT ( 'NONE',  ( 30.37540678000427619, 0.000000000000000000, 7.500000000000000000 ) ) ;
#4230 = CIRCLE ( 'NONE', #3511, 5.300000000000006040 ) ;
#4231 = AXIS2_PLACEMENT_3D ( 'NONE', #14290, #10830, #5713 ) ;
#4232 = EDGE_LOOP ( 'NONE', ( #1655, #12286, #1367, #7456 ) ) ;
#4233 = EDGE_CURVE ( 'NONE', #7404, #1516, #3502, .T. ) ;
#4234 = ADVANCED_FACE ( 'NONE', ( #8698 ), #12406, .F. ) ;
#4235 = AXIS2_PLACEMENT_3D ( 'NONE', #424, #15643, #526 ) ;
#4236 = EDGE_LOOP ( 'NONE', ( #10803, #8417, #14392, #7189 ) ) ;
#4237 = AXIS2_PLACEMENT_3D ( 'NONE', #15451, #120, #6969 ) ;
#4238 = CIRCLE ( 'NONE', #18891, 0.2999999999999947153 ) ;
#4239 = ORIENTED_EDGE ( 'NONE', *, *, #18724, .T. ) ;
#4240 = CYLINDRICAL_SURFACE ( 'NONE', #11709, 5.000000000000004441 ) ;
#4241 = CARTESIAN_POINT ( 'NONE',  ( 34.99999999999999289, -84.70000000000001705, 79.39999999999999147 ) ) ;
#4242 = CARTESIAN_POINT ( 'NONE',  ( 15.21174975910707161, 51.61873716947361856, 68.25000000000000000 ) ) ;
#4243 = DIRECTION ( 'NONE',  ( 1.000000000000000000, 0.000000000000000000, 0.000000000000000000 ) ) ;
#4244 = CARTESIAN_POINT ( 'NONE',  ( -14.71174975910705029, 50.19799549595485644, 68.50000000000000000 ) ) ;
#4245 = VERTEX_POINT ( 'NONE', #385 ) ;
#4246 = CIRCLE ( 'NONE', #22116, 3.017785046117004377 ) ;
#4247 = CARTESIAN_POINT ( 'NONE',  ( -28.87540678000427619, -6.494748934539263274, 13.19999999999999929 ) ) ;
#4248 = CYLINDRICAL_SURFACE ( 'NONE', #14979, 0.2500000000000001665 ) ;
#4249 = CIRCLE ( 'NONE', #19611, 5.000000000000004441 ) ;
#4250 = CARTESIAN_POINT ( 'NONE',  ( 1.774728116533979883, 42.36054587065083155, 37.66679706732590915 ) ) ;
#4251 = PRODUCT_DEFINITION ( 'UNKNOWN', '', #11935, #18704 ) ;
#4252 = AXIS2_PLACEMENT_3D ( 'NONE', #20744, #3726, #10875 ) ;
#4253 = CARTESIAN_POINT ( 'NONE',  ( -24.69594744299175915, 42.46645089659918426, 13.74999999999999822 ) ) ;
#4254 = VERTEX_POINT ( 'NONE', #21288 ) ;
#4255 = ORIENTED_EDGE ( 'NONE', *, *, #9755, .F. ) ;
#4256 = LINE ( 'NONE', #17889, #9959 ) ;
#4257 = PRODUCT_CONTEXT ( 'NONE', #5452, 'mechanical' ) ;
#4258 = ORIENTED_EDGE ( 'NONE', *, *, #8634, .T. ) ;
#4259 = EDGE_LOOP ( 'NONE', ( #2461, #19521, #926, #13192 ) ) ;
#4260 = EDGE_CURVE ( 'NONE', #21299, #15569, #12026, .T. ) ;
#4261 = B_SPLINE_CURVE_WITH_KNOTS ( 'NONE', 3,
 ( #2383, #16658, #1337, #6518, #2271, #1007, #20048, #18346, #9214, #21097, #19398, #16329 ),
 .UNSPECIFIED., .F., .F.,
 ( 4, 2, 2, 2, 2, 4 ),
 ( 0.000000000000000000, 0.0006847042422322839909, 0.001027056363348426583, 0.001198232423906498041, 0.001283820454185535071, 0.001369408484464571885 ),
 .UNSPECIFIED. ) ;
#4262 = DIRECTION ( 'NONE',  ( 0.000000000000000000, 0.000000000000000000, 1.000000000000000000 ) ) ;
#4263 = ORIENTED_EDGE ( 'NONE', *, *, #7348, .T. ) ;
#4264 = DIRECTION ( 'NONE',  ( 0.000000000000000000, -0.000000000000000000, 1.000000000000000000 ) ) ;
#4265 = ORIENTED_EDGE ( 'NONE', *, *, #11947, .F. ) ;
#4266 = AXIS2_PLACEMENT_3D ( 'NONE', #19797, #1101, #19568 ) ;
#4267 = CARTESIAN_POINT ( 'NONE',  ( 27.77120804565220169, -2.094189496455408861, -150.0833101980363722 ) ) ;
#4268 = CARTESIAN_POINT ( 'NONE',  ( 29.69597781366221767, 56.94165929845684104, 70.50000000000000000 ) ) ;
#4269 = DIRECTION ( 'NONE',  ( 0.000000000000000000, 0.000000000000000000, 1.000000000000000000 ) ) ;
#4270 = DIRECTION ( 'NONE',  ( 0.000000000000000000, 0.000000000000000000, 1.000000000000000000 ) ) ;
#4271 = CARTESIAN_POINT ( 'NONE',  ( -14.96174975910705207, 50.19799549595485644, -3.500000000000003109 ) ) ;
#4272 = DIRECTION ( 'NONE',  ( 0.000000000000000000, 0.000000000000000000, 1.000000000000000000 ) ) ;
#4274 = EDGE_CURVE ( 'NONE', #1545, #2819, #12753, .T. ) ;
#4273 = CARTESIAN_POINT ( 'NONE',  ( -33.20000000000001705, 85.00000000000000000, 78.20000000000000284 ) ) ;
#4275 = CARTESIAN_POINT ( 'NONE',  ( -1.774728116533986766, 42.36054587065083155, 51.80876104995653719 ) ) ;
#4276 = AXIS2_PLACEMENT_3D ( 'NONE', #12942, #2776, #21592 ) ;
#4277 = AXIS2_PLACEMENT_3D ( 'NONE', #18951, #13672, #10446 ) ;
#4278 = VECTOR ( 'NONE', #1554, 1000.000000000000000 ) ;
#4279 = CARTESIAN_POINT ( 'NONE',  ( -8.638906393579159015, 43.26651812033729527, 68.06527860057354928 ) ) ;
#4280 = ORIENTED_EDGE ( 'NONE', *, *, #1060, .F. ) ;
#4281 = ORIENTED_EDGE ( 'NONE', *, *, #12598, .T. ) ;
#4282 = CARTESIAN_POINT ( 'NONE',  ( -15.21174975910705207, 51.61873716947361856, 68.25000000000000000 ) ) ;
#4283 = EDGE_CURVE ( 'NONE', #8087, #11459, #16072, .T. ) ;
#4284 = ADVANCED_FACE ( 'NONE', ( #73 ), #8794, .T. ) ;
#4285 = ORIENTED_EDGE ( 'NONE', *, *, #15925, .T. ) ;
#4286 = AXIS2_PLACEMENT_3D ( 'NONE', #22017, #5233, #8596 ) ;
#4287 = AXIS2_PLACEMENT_3D ( 'NONE', #8602, #22151, #15175 ) ;
#4288 = DIRECTION ( 'NONE',  ( 0.000000000000000000, -0.000000000000000000, -1.000000000000000000 ) ) ;
#4289 = AXIS2_PLACEMENT_3D ( 'NONE', #12446, #19177, #17603 ) ;
#4290 = CARTESIAN_POINT ( 'NONE',  ( -1.824728116533986810, 42.36054587065083155, 35.75876104995654003 ) ) ;
#4291 = ORIENTED_EDGE ( 'NONE', *, *, #2277, .T. ) ;
#4292 = PRESENTATION_STYLE_ASSIGNMENT (( #19619 ) ) ;
#4293 = EDGE_CURVE ( 'NONE', #8378, #8119, #5307, .T. ) ;
#4294 = DIRECTION ( 'NONE',  ( -0.000000000000000000, -0.000000000000000000, -1.000000000000000000 ) ) ;
#4295 = CARTESIAN_POINT ( 'NONE',  ( -1.724728116533986721, 42.36054587065083155, 45.66679706732590205 ) ) ;
#4296 = CARTESIAN_POINT ( 'NONE',  ( 1.824728116533979705, 42.36054587065083155, 53.66679706732590915 ) ) ;
#4297 = CARTESIAN_POINT ( 'NONE',  ( 31.44597781366222122, 56.94165929845684104, 70.50000000000000000 ) ) ;
#4298 = ORIENTED_EDGE ( 'NONE', *, *, #16381, .T. ) ;
#4299 = CARTESIAN_POINT ( 'NONE',  ( 28.64417692495746692, -6.713479613976641502, 13.50000000000000000 ) ) ;
#4300 = DIRECTION ( 'NONE',  ( 0.000000000000000000, -0.000000000000000000, 1.000000000000000000 ) ) ;
#4301 = CARTESIAN_POINT ( 'NONE',  ( 29.69597781366221767, 27.99124249474150972, 70.50000000000000000 ) ) ;
#4302 = ORIENTED_EDGE ( 'NONE', *, *, #17016, .T. ) ;
#4303 = EDGE_LOOP ( 'NONE', ( #2109, #8572, #3518, #10200 ) ) ;
#4304 = EDGE_LOOP ( 'NONE', ( #2472, #19545, #17213, #17566 ) ) ;
#4305 = DIRECTION ( 'NONE',  ( 0.000000000000000000, 0.000000000000000000, -1.000000000000000000 ) ) ;
#4306 = AXIS2_PLACEMENT_3D ( 'NONE', #1834, #8675, #20190 ) ;
#4307 = FACE_OUTER_BOUND ( 'NONE', #10750, .T. ) ;
#4308 = EDGE_CURVE ( 'NONE', #1591, #5684, #19086, .T. ) ;
#4309 = ORIENTED_EDGE ( 'NONE', *, *, #2603, .T. ) ;
#4310 = VECTOR ( 'NONE', #14656, 1000.000000000000000 ) ;
#4311 = EDGE_CURVE ( 'NONE', #12515, #7899, #18873, .T. ) ;
#4312 = CARTESIAN_POINT ( 'NONE',  ( -35.00000000000001421, 85.00000000000000000, 80.00000000000000000 ) ) ;
#4313 = EDGE_CURVE ( 'NONE', #7362, #97, #5655, .T. ) ;
#4314 = ORIENTED_EDGE ( 'NONE', *, *, #11025, .F. ) ;
#4315 = CARTESIAN_POINT ( 'NONE',  ( 0.000000000000000000, 0.000000000000000000, 13.50000000000000000 ) ) ;
#4316 = CARTESIAN_POINT ( 'NONE',  ( -1.774728116533986766, 42.31054587065082728, 33.66679706732590915 ) ) ;
#4317 = FACE_OUTER_BOUND ( 'NONE', #10397, .T. ) ;
#4318 = DIRECTION ( 'NONE',  ( -1.000000000000000000, 0.000000000000000000, 0.000000000000000000 ) ) ;
#4319 = DIRECTION ( 'NONE',  ( -2.388292521039847891E-16, -0.000000000000000000, -1.000000000000000000 ) ) ;
#4320 = DIRECTION ( 'NONE',  ( -0.000000000000000000, 1.000000000000000000, 0.000000000000000000 ) ) ;
#4321 = ORIENTED_EDGE ( 'NONE', *, *, #8838, .F. ) ;
#4322 = FACE_OUTER_BOUND ( 'NONE', #12132, .T. ) ;
#4323 = LINE ( 'NONE', #7478, #17466 ) ;
#4324 = ADVANCED_FACE ( 'NONE', ( #17394 ), #277, .T. ) ;
#4325 = VECTOR ( 'NONE', #969, 1000.000000000000000 ) ;
#4326 = DIRECTION ( 'NONE',  ( -0.000000000000000000, -0.000000000000000000, -1.000000000000000000 ) ) ;
#4327 = CARTESIAN_POINT ( 'NONE',  ( 30.19999999999999574, 70.29999999999999716, 1.200000000000003952 ) ) ;
#4328 = ORIENTED_EDGE ( 'NONE', *, *, #13137, .T. ) ;
#4329 = DIRECTION ( 'NONE',  ( 6.123233995736764803E-17, -0.000000000000000000, -1.000000000000000000 ) ) ;
#4330 = CARTESIAN_POINT ( 'NONE',  ( -15.21174975910705207, 41.81054587065082728, 68.50000000000000000 ) ) ;
#4331 = EDGE_LOOP ( 'NONE', ( #16767, #7747, #1634, #11147 ) ) ;
#4332 = DIRECTION ( 'NONE',  ( 0.000000000000000000, -1.000000000000000000, 0.000000000000000000 ) ) ;
#4333 = DIRECTION ( 'NONE',  ( 1.000000000000000000, 0.000000000000000000, 0.000000000000000000 ) ) ;
#4334 = VERTEX_POINT ( 'NONE', #8908 ) ;
#4335 = ORIENTED_EDGE ( 'NONE', *, *, #19403, .F. ) ;
#4336 = CARTESIAN_POINT ( 'NONE',  ( -29.20000000000002061, 68.70000000000001705, 0.000000000000000000 ) ) ;
#4337 = CARTESIAN_POINT ( 'NONE',  ( -34.39999999999999858, 85.00000000000000000, 0.3000000000000000444 ) ) ;
#4338 = AXIS2_PLACEMENT_3D ( 'NONE', #7681, #17415, #17632 ) ;
#4339 = DIRECTION ( 'NONE',  ( 1.000000000000000000, 2.105859220307292343E-16, -0.000000000000000000 ) ) ;
#4340 = VECTOR ( 'NONE', #13696, 1000.000000000000000 ) ;
#4341 = ADVANCED_FACE ( 'NONE', ( #15714 ), #7237, .F. ) ;
#4342 = ORIENTED_EDGE ( 'NONE', *, *, #5559, .T. ) ;
#4343 = ADVANCED_FACE ( 'NONE', ( #11530 ), #16673, .T. ) ;
#4344 = CIRCLE ( 'NONE', #1424, 0.2999999999999947153 ) ;
#4345 = EDGE_LOOP ( 'NONE', ( #1134, #1048, #9718, #6847 ) ) ;
#4346 = CARTESIAN_POINT ( 'NONE',  ( -8.641460742840918030, 33.93424481021354921, 68.50000000000000000 ) ) ;
#4347 = DIRECTION ( 'NONE',  ( 1.000000000000000000, 0.000000000000000000, 0.000000000000000000 ) ) ;
#4348 = DIRECTION ( 'NONE',  ( 0.000000000000000000, -1.000000000000000000, 0.000000000000000000 ) ) ;
#4349 = VECTOR ( 'NONE', #475, 1000.000000000000000 ) ;
#4350 = PLANE ( 'NONE',  #18218 ) ;
#4351 = CARTESIAN_POINT ( 'NONE',  ( 32.20000000000001705, 71.00000000000001421, 3.500000000000000000 ) ) ;
#4352 = DIRECTION ( 'NONE',  ( 0.000000000000000000, 1.000000000000000000, 0.000000000000000000 ) ) ;
#4353 = AXIS2_PLACEMENT_3D ( 'NONE', #6888, #20518, #12107 ) ;
#4354 = DIRECTION ( 'NONE',  ( -0.000000000000000000, -1.000000000000000000, 0.000000000000000000 ) ) ;
#4355 = CARTESIAN_POINT ( 'NONE',  ( -30.49999999999999289, -84.70000000000001705, -1.716353773989596664E-15 ) ) ;
#4356 = ORIENTED_EDGE ( 'NONE', *, *, #9644, .T. ) ;
#4357 = CYLINDRICAL_SURFACE ( 'NONE', #896, 0.3000000000000016542 ) ;
#4358 = EDGE_CURVE ( 'NONE', #2540, #16676, #4616, .T. ) ;
#4359 = DIRECTION ( 'NONE',  ( 0.000000000000000000, 0.000000000000000000, -1.000000000000000000 ) ) ;
#4360 = CARTESIAN_POINT ( 'NONE',  ( -17.95292532278785913, -34.11873716947361856, 68.00000000000000000 ) ) ;
#4361 = CARTESIAN_POINT ( 'NONE',  ( 1.824728116533979705, 42.36054587065083155, 49.66679706732590915 ) ) ;
#4362 = ORIENTED_EDGE ( 'NONE', *, *, #4743, .T. ) ;
#4363 = ORIENTED_EDGE ( 'NONE', *, *, #21144, .T. ) ;
#4364 = DIRECTION ( 'NONE',  ( -1.000000000000000000, 0.000000000000000000, 0.000000000000000000 ) ) ;
#4365 = EDGE_CURVE ( 'NONE', #852, #16858, #14886, .T. ) ;
#4366 = AXIS2_PLACEMENT_3D ( 'NONE', #18801, #3145, #11855 ) ;
#4367 = ORIENTED_EDGE ( 'NONE', *, *, #4785, .F. ) ;
#4368 = AXIS2_PLACEMENT_3D ( 'NONE', #14298, #5824, #19562 ) ;
#4369 = ORIENTED_EDGE ( 'NONE', *, *, #17605, .T. ) ;
#4370 = CARTESIAN_POINT ( 'NONE',  ( 27.67540678000429111, -36.74634676501047181, 13.50000000000000000 ) ) ;
#4371 = EDGE_LOOP ( 'NONE', ( #21084, #6360, #7295, #4438 ) ) ;
#4372 = LINE ( 'NONE', #6995, #15021 ) ;
#4373 = ORIENTED_EDGE ( 'NONE', *, *, #19179, .T. ) ;
#4374 = CYLINDRICAL_SURFACE ( 'NONE', #3449, 0.2999999999999999334 ) ;
#4375 = DIRECTION ( 'NONE',  ( 0.000000000000000000, 0.000000000000000000, 1.000000000000000000 ) ) ;
#4376 = DIRECTION ( 'NONE',  ( -0.000000000000000000, -1.000000000000000000, -0.000000000000000000 ) ) ;
#4377 = ADVANCED_FACE ( 'NONE', ( #20159 ), #3036, .T. ) ;
#4378 = CARTESIAN_POINT ( 'NONE',  ( -27.37540678000427974, -5.683640910026986681, 13.79999999999999893 ) ) ;
#4379 = VECTOR ( 'NONE', #3643, 1000.000000000000000 ) ;
#4380 = DIRECTION ( 'NONE',  ( -0.000000000000000000, 0.000000000000000000, 1.000000000000000000 ) ) ;
#4381 = EDGE_CURVE ( 'NONE', #8265, #21066, #12869, .T. ) ;
#4382 = CYLINDRICAL_SURFACE ( 'NONE', #873, 0.2999999999999947153 ) ;
#4383 = VERTEX_POINT ( 'NONE', #19720 ) ;
#4384 = CARTESIAN_POINT ( 'NONE',  ( -23.33295178540679160, 45.13732965806239150, 68.25000000000000000 ) ) ;
#4385 = CARTESIAN_POINT ( 'NONE',  ( -23.32398829872514057, 7.118794219358020148E-15, 13.50000000000000000 ) ) ;
#4386 = ORIENTED_EDGE ( 'NONE', *, *, #10908, .F. ) ;
#4387 = ORIENTED_EDGE ( 'NONE', *, *, #12213, .T. ) ;
#4388 = CARTESIAN_POINT ( 'NONE',  ( 15.95292532278785913, 51.61873716947361856, 68.50000000000000000 ) ) ;
#4389 = AXIS2_PLACEMENT_3D ( 'NONE', #236, #8758, #7302 ) ;
#4390 = ORIENTED_EDGE ( 'NONE', *, *, #10868, .T. ) ;
#4391 = ORIENTED_EDGE ( 'NONE', *, *, #12969, .T. ) ;
#4392 = VERTEX_POINT ( 'NONE', #4824 ) ;
#4393 = ADVANCED_FACE ( 'NONE', ( #9865 ), #10298, .T. ) ;
#4394 = VERTEX_POINT ( 'NONE', #21743 ) ;
#4395 = DIRECTION ( 'NONE',  ( -1.000000000000000000, 0.000000000000000000, 0.000000000000000000 ) ) ;
#4396 = ORIENTED_EDGE ( 'NONE', *, *, #20754, .F. ) ;
#4397 = CARTESIAN_POINT ( 'NONE',  ( 1.724728116533979616, 42.36054587065083155, 41.76679706732590347 ) ) ;
#4398 = EDGE_CURVE ( 'NONE', #16055, #15493, #10639, .T. ) ;
#4399 = PLANE ( 'NONE',  #11120 ) ;
#4400 = CARTESIAN_POINT ( 'NONE',  ( -6.728906393579157097, 41.92645089659919933, 70.88527860057354246 ) ) ;
#4401 = CARTESIAN_POINT ( 'NONE',  ( -29.69597781366221412, 27.99124249474150972, 70.50000000000000000 ) ) ;
#4402 = DIRECTION ( 'NONE',  ( 1.000000000000000000, 0.000000000000000000, 0.000000000000000000 ) ) ;
#4403 = ORIENTED_EDGE ( 'NONE', *, *, #20998, .T. ) ;
#4404 = CARTESIAN_POINT ( 'NONE',  ( 15.21174975910705918, -41.81054587065082728, 13.79999999999999893 ) ) ;
#4405 = DIRECTION ( 'NONE',  ( -1.224646799147353207E-16, -0.000000000000000000, -1.000000000000000000 ) ) ;
#4406 = ORIENTED_EDGE ( 'NONE', *, *, #21806, .F. ) ;
#4407 = ORIENTED_EDGE ( 'NONE', *, *, #17189, .F. ) ;
#4408 = ORIENTED_EDGE ( 'NONE', *, *, #7023, .F. ) ;
#4409 = CARTESIAN_POINT ( 'NONE',  ( 31.50000000000002132, -71.00000000000001421, 3.200000000000000178 ) ) ;
#4410 = DIRECTION ( 'NONE',  ( -2.107255972849994642E-16, 0.000000000000000000, -1.000000000000000000 ) ) ;
#4411 = ORIENTED_EDGE ( 'NONE', *, *, #10122, .F. ) ;
#4412 = CARTESIAN_POINT ( 'NONE',  ( 27.37540678000428684, -36.74634676501047181, 42.50000000000000000 ) ) ;
#4413 = EDGE_CURVE ( 'NONE', #17830, #6609, #9209, .T. ) ;
#4414 = ORIENTED_EDGE ( 'NONE', *, *, #21321, .F. ) ;
#4415 = DIRECTION ( 'NONE',  ( -1.000000000000000000, 0.000000000000000000, 0.000000000000000000 ) ) ;
#4416 = CARTESIAN_POINT ( 'NONE',  ( -17.45292532278785913, -38.74634676501045760, 13.99999999999999822 ) ) ;
#4417 = DIRECTION ( 'NONE',  ( 0.000000000000000000, 0.000000000000000000, 1.000000000000000000 ) ) ;
#4418 = DIRECTION ( 'NONE',  ( -1.000000000000000000, 0.000000000000000000, 0.000000000000000000 ) ) ;
#4419 = CARTESIAN_POINT ( 'NONE',  ( 33.19999999999999574, 84.70000000000001705, 1.799999999999996048 ) ) ;
#4420 = DIRECTION ( 'NONE',  ( 1.000000000000000000, 0.000000000000000000, 0.000000000000000000 ) ) ;
#4421 = ORIENTED_EDGE ( 'NONE', *, *, #16881, .T. ) ;
#4422 = CARTESIAN_POINT ( 'NONE',  ( 1.724728116533979616, 42.31054587065082728, 39.80876104995653719 ) ) ;
#4423 = CARTESIAN_POINT ( 'NONE',  ( -14.83748569039512155, 41.93480993936275070, 13.50000000000000000 ) ) ;
#4424 = EDGE_CURVE ( 'NONE', #4126, #19345, #14201, .T. ) ;
#4425 = ADVANCED_FACE ( 'NONE', ( #2596 ), #15010, .T. ) ;
#4426 = CIRCLE ( 'NONE', #3713, 1.500000000000001332 ) ;
#4427 = ADVANCED_FACE ( 'NONE', ( #16342 ), #2693, .T. ) ;
#4428 = CARTESIAN_POINT ( 'NONE',  ( -27.67540678000427690, 10.94079601157914539, 13.50000000000000000 ) ) ;
#4429 = CARTESIAN_POINT ( 'NONE',  ( 30.07540678000427548, 63.74634676501045050, 7.500000000000000000 ) ) ;
#4430 = ORIENTED_EDGE ( 'NONE', *, *, #10623, .T. ) ;
#4431 = PRESENTATION_STYLE_ASSIGNMENT (( #14382 ) ) ;
#4432 = DIRECTION ( 'NONE',  ( -0.000000000000000000, -0.000000000000000000, -1.000000000000000000 ) ) ;
#4433 = VERTEX_POINT ( 'NONE', #13217 ) ;
#4434 = CYLINDRICAL_SURFACE ( 'NONE', #13041, 0.5000000000000004441 ) ;
#4435 = CIRCLE ( 'NONE', #9432, 0.5000000000000004441 ) ;
#4436 = CARTESIAN_POINT ( 'NONE',  ( 29.13662752439705272, 4.700000000000000178, 3.799999999999999822 ) ) ;
#4437 = ORIENTED_EDGE ( 'NONE', *, *, #3620, .T. ) ;
#4438 = ORIENTED_EDGE ( 'NONE', *, *, #6555, .T. ) ;
#4439 = DIRECTION ( 'NONE',  ( -0.9823853469773031755, -0.1868663427273193067, -0.000000000000000000 ) ) ;
#4440 = CARTESIAN_POINT ( 'NONE',  ( 17.92752199202934094, -50.11873716947361856, 13.79999999999999893 ) ) ;
#4441 = DIRECTION ( 'NONE',  ( 0.000000000000000000, 0.000000000000000000, -1.000000000000000000 ) ) ;
#4442 = ORIENTED_EDGE ( 'NONE', *, *, #169, .F. ) ;
#4443 = EDGE_CURVE ( 'NONE', #20393, #2605, #16218, .T. ) ;
#4444 = ORIENTED_EDGE ( 'NONE', *, *, #7123, .T. ) ;
#4445 = CARTESIAN_POINT ( 'NONE',  ( -4.985331397971318523, 42.46645089659917716, 70.50000000000000000 ) ) ;
#4446 = CARTESIAN_POINT ( 'NONE',  ( -14.96174975910705385, -41.81054587065082728, 13.62426406871192874 ) ) ;
#4447 = CARTESIAN_POINT ( 'NONE',  ( -23.02398829872513986, -2.333317872336245102, 13.47139736055071602 ) ) ;
#4448 = CARTESIAN_POINT ( 'NONE',  ( -1.824728116533986810, 43.31054587065082728, 27.70876104995653577 ) ) ;
#4449 = LINE ( 'NONE', #11263, #17491 ) ;
#4450 = DIRECTION ( 'NONE',  ( 0.000000000000000000, 0.000000000000000000, 1.000000000000000000 ) ) ;
#4451 = DIRECTION ( 'NONE',  ( -0.2309407893632008379, 0.9729678061520339316, 0.000000000000000000 ) ) ;
#4452 = EDGE_CURVE ( 'NONE', #12093, #7942, #16458, .T. ) ;
#4453 = EDGE_CURVE ( 'NONE', #8198, #20854, #21368, .T. ) ;
#4454 = CARTESIAN_POINT ( 'NONE',  ( -29.50000000000002132, -69.00000000000000000, 0.2999999999999947153 ) ) ;
#4455 = PRODUCT_DEFINITION_SHAPE ( 'NONE', 'NONE',  #22178 ) ;
#4456 = FACE_OUTER_BOUND ( 'NONE', #4491, .T. ) ;
#4457 = ORIENTED_EDGE ( 'NONE', *, *, #12598, .F. ) ;
#4458 = CARTESIAN_POINT ( 'NONE',  ( 29.69597781366221767, 58.69165929845684104, 70.25000000000000000 ) ) ;
#4459 = EDGE_CURVE ( 'NONE', #10145, #20423, #19947, .T. ) ;
#4460 = DIRECTION ( 'NONE',  ( 0.000000000000000000, 0.000000000000000000, 1.000000000000000000 ) ) ;
#4461 = CARTESIAN_POINT ( 'NONE',  ( 15.21174975910707161, 42.31054587065082728, 68.25000000000000000 ) ) ;
#4462 = ORIENTED_EDGE ( 'NONE', *, *, #15105, .F. ) ;
#4463 = DIRECTION ( 'NONE',  ( -0.000000000000000000, -0.000000000000000000, -1.000000000000000000 ) ) ;
#4464 = DIRECTION ( 'NONE',  ( 0.000000000000000000, 0.000000000000000000, 1.000000000000000000 ) ) ;
#4465 = EDGE_LOOP ( 'NONE', ( #8800, #9501, #14164, #15015 ) ) ;
#4466 = CIRCLE ( 'NONE', #10897, 0.05000000000000143219 ) ;
#4467 = ORIENTED_EDGE ( 'NONE', *, *, #9413, .F. ) ;
#4468 = CARTESIAN_POINT ( 'NONE',  ( 33.79999999999999005, -85.00000000000000000, 78.20000000000000284 ) ) ;
#4469 = ADVANCED_FACE ( 'NONE', ( #13092 ), #1230, .T. ) ;
#4470 = EDGE_LOOP ( 'NONE', ( #19739, #11241, #10232, #12594 ) ) ;
#4471 = EDGE_CURVE ( 'NONE', #21679, #6512, #3521, .T. ) ;
#4472 = DIRECTION ( 'NONE',  ( 0.000000000000000000, 1.000000000000000000, 0.000000000000000000 ) ) ;
#4473 = CYLINDRICAL_SURFACE ( 'NONE', #15251, 0.5000000000000004441 ) ;
#4474 = ORIENTED_EDGE ( 'NONE', *, *, #7259, .F. ) ;
#4475 = LINE ( 'NONE', #4267, #6669 ) ;
#4476 = CARTESIAN_POINT ( 'NONE',  ( 29.50000000000002132, 0.000000000000000000, -150.0833101980363722 ) ) ;
#4477 = DIRECTION ( 'NONE',  ( 1.000000000000000000, 0.000000000000000000, 0.000000000000000000 ) ) ;
#4478 = DIRECTION ( 'NONE',  ( -0.000000000000000000, -0.000000000000000000, -1.000000000000000000 ) ) ;
#4479 = AXIS2_PLACEMENT_3D ( 'NONE', #14253, #17278, #21103 ) ;
#4480 = VECTOR ( 'NONE', #2753, 1000.000000000000000 ) ;
#4481 = LINE ( 'NONE', #21732, #3967 ) ;
#4482 = EDGE_CURVE ( 'NONE', #3240, #10960, #21384, .T. ) ;
#4483 = CARTESIAN_POINT ( 'NONE',  ( 1.724728116533979838, 43.31054587065082728, 49.71679706732589921 ) ) ;
#4484 = DIRECTION ( 'NONE',  ( 0.000000000000000000, 0.000000000000000000, 1.000000000000000000 ) ) ;
#4485 = CARTESIAN_POINT ( 'NONE',  ( -30.49999999999999289, -84.70000000000001705, 1.199999999999999734 ) ) ;
#4486 = EDGE_LOOP ( 'NONE', ( #8604, #16189, #4915, #11217 ) ) ;
#4487 = DIRECTION ( 'NONE',  ( 1.000000000000000000, 0.000000000000000000, 0.000000000000000000 ) ) ;
#4488 = DIRECTION ( 'NONE',  ( -0.000000000000000000, 0.000000000000000000, 1.000000000000000000 ) ) ;
#4489 = ORIENTED_EDGE ( 'NONE', *, *, #21414, .T. ) ;
#4490 = MECHANICAL_DESIGN_GEOMETRIC_PRESENTATION_REPRESENTATION (  '', ( #18052 ), #8424 ) ;
#4491 = EDGE_LOOP ( 'NONE', ( #11357, #12934, #9710, #16876 ) ) ;
#4492 = CARTESIAN_POINT ( 'NONE',  ( 0.000000000000000000, -32.11873716947361856, 42.50000000000000711 ) ) ;
#4493 = CIRCLE ( 'NONE', #21664, 0.2999999999999999334 ) ;
#4494 = AXIS2_PLACEMENT_3D ( 'NONE', #8367, #11929, #8710 ) ;
#4495 = VERTEX_POINT ( 'NONE', #6631 ) ;
#4496 = EDGE_CURVE ( 'NONE', #2381, #11265, #8403, .T. ) ;
#4497 = ADVANCED_FACE ( 'NONE', ( #8525 ), #8870, .T. ) ;
#4498 = EDGE_CURVE ( 'NONE', #689, #8585, #117, .T. ) ;
#4499 = EDGE_LOOP ( 'NONE', ( #10039, #16415, #1081, #17117 ) ) ;
#4500 = CARTESIAN_POINT ( 'NONE',  ( 14.90249074828138198, -52.32070855728485981, 13.50000000000000000 ) ) ;
#4501 = AXIS2_PLACEMENT_3D ( 'NONE', #19938, #9641, #18241 ) ;
#4502 = AXIS2_PLACEMENT_3D ( 'NONE', #303, #13836, #2096 ) ;
#4503 = CYLINDRICAL_SURFACE ( 'NONE', #18438, 0.05000000000000143219 ) ;
#4504 = CIRCLE ( 'NONE', #18792, 0.05000000000000143219 ) ;
#4505 = VERTEX_POINT ( 'NONE', #15339 ) ;
#4506 = DIRECTION ( 'NONE',  ( 0.000000000000000000, 1.000000000000000000, 0.000000000000000000 ) ) ;
#4507 = CARTESIAN_POINT ( 'NONE',  ( -35.00000000000001421, 84.70000000000001705, 80.00000000000000000 ) ) ;
#4508 = CARTESIAN_POINT ( 'NONE',  ( -15.95292532278785913, 50.11873716947361856, 13.99999999999999822 ) ) ;
#4509 = CARTESIAN_POINT ( 'NONE',  ( -23.32398829872514057, 3.528912754968630328, 13.50000000000000000 ) ) ;
#4510 = AXIS2_PLACEMENT_3D ( 'NONE', #9670, #13231, #14903 ) ;
#4511 = ORIENTED_EDGE ( 'NONE', *, *, #13957, .F. ) ;
#4512 = LINE ( 'NONE', #21875, #17221 ) ;
#4513 = LINE ( 'NONE', #19629, #9853 ) ;
#4514 = ORIENTED_EDGE ( 'NONE', *, *, #10465, .F. ) ;
#4515 = EDGE_CURVE ( 'NONE', #21509, #22135, #16000, .T. ) ;
#4516 = ORIENTED_EDGE ( 'NONE', *, *, #8456, .F. ) ;
#4517 = ORIENTED_EDGE ( 'NONE', *, *, #5530, .F. ) ;
#4518 = CARTESIAN_POINT ( 'NONE',  ( 0.000000000000000000, 4.700000000000000178, 3.500000000000000000 ) ) ;
#4519 = ORIENTED_EDGE ( 'NONE', *, *, #5723, .F. ) ;
#4520 = VECTOR ( 'NONE', #17622, 1000.000000000000000 ) ;
#4521 = AXIS2_PLACEMENT_3D ( 'NONE', #16051, #17529, #7357 ) ;
#4522 = TOROIDAL_SURFACE ( 'NONE', #15945, 1.500000000000000000, 0.5000000000000000000 ) ;
#4523 = DIRECTION ( 'NONE',  ( 1.000000000000000000, 0.000000000000000000, 0.000000000000000000 ) ) ;
#4524 = CIRCLE ( 'NONE', #7745, 0.3000000000000003775 ) ;
#4525 = EDGE_CURVE ( 'NONE', #3080, #9063, #2746, .T. ) ;
#4526 = VERTEX_POINT ( 'NONE', #13019 ) ;
#4527 = LINE ( 'NONE', #7671, #13926 ) ;
#4528 = EDGE_CURVE ( 'NONE', #11049, #6609, #4238, .T. ) ;
#4529 = AXIS2_PLACEMENT_3D ( 'NONE', #14664, #894, #17911 ) ;
#4530 = CARTESIAN_POINT ( 'NONE',  ( 1.774728116533979438, 43.31054587065082728, 39.80876104995653719 ) ) ;
#4531 = CARTESIAN_POINT ( 'NONE',  ( 23.02398829872514341, -3.262290859344324723, 13.80000000000000071 ) ) ;
#4532 = CARTESIAN_POINT ( 'NONE',  ( 15.95292532278785913, -32.11873716947361856, 68.00000000000000000 ) ) ;
#4533 = CARTESIAN_POINT ( 'NONE',  ( 29.69597781366221767, 56.94165929845684104, 68.50000000000000000 ) ) ;
#4534 = CARTESIAN_POINT ( 'NONE',  ( -1.824728116533986810, 42.36054587065083155, 29.76679706732590702 ) ) ;
#4535 = ORIENTED_EDGE ( 'NONE', *, *, #16088, .F. ) ;
#4536 = FACE_OUTER_BOUND ( 'NONE', #18518, .T. ) ;
#4537 = FACE_OUTER_BOUND ( 'NONE', #7571, .T. ) ;
#4538 = VECTOR ( 'NONE', #10237, 1000.000000000000000 ) ;
#4539 = DIRECTION ( 'NONE',  ( -0.000000000000000000, 1.000000000000000000, -0.000000000000000000 ) ) ;
#4540 = CARTESIAN_POINT ( 'NONE',  ( -32.23382792203229741, 83.71979900898287497, 68.25000000000000000 ) ) ;
#4541 = DIRECTION ( 'NONE',  ( 0.000000000000000000, -0.000000000000000000, 1.000000000000000000 ) ) ;
#4542 = ORIENTED_EDGE ( 'NONE', *, *, #7809, .T. ) ;
#4543 = CIRCLE ( 'NONE', #18109, 0.04999999999999991257 ) ;
#4544 = AXIS2_PLACEMENT_3D ( 'NONE', #17179, #10692, #159 ) ;
#4545 = SURFACE_SIDE_STYLE ('',( #7586 ) ) ;
#4546 = CARTESIAN_POINT ( 'NONE',  ( 17.45292532278785913, -50.11873716947361856, 14.00000000000000000 ) ) ;
#4547 = AXIS2_PLACEMENT_3D ( 'NONE', #16757, #8609, #3337 ) ;
#4548 = ORIENTED_EDGE ( 'NONE', *, *, #12903, .T. ) ;
#4549 = DIRECTION ( 'NONE',  ( 2.107255972849994642E-16, 0.000000000000000000, 1.000000000000000000 ) ) ;
#4550 = CIRCLE ( 'NONE', #17048, 0.2999999999999999334 ) ;
#4551 = CARTESIAN_POINT ( 'NONE',  ( -9.641460742840918030, 32.61873716947361856, 42.50000000000000711 ) ) ;
#4552 = ORIENTED_EDGE ( 'NONE', *, *, #2999, .F. ) ;
#4553 = EDGE_LOOP ( 'NONE', ( #106, #5224, #17633, #17602 ) ) ;
#4554 = AXIS2_PLACEMENT_3D ( 'NONE', #6584, #20010, #11483 ) ;
#4555 = ORIENTED_EDGE ( 'NONE', *, *, #7972, .F. ) ;
#4556 = DIRECTION ( 'NONE',  ( 1.000000000000000000, 0.000000000000000000, -0.000000000000000000 ) ) ;
#4557 = CARTESIAN_POINT ( 'NONE',  ( -1.824728116533986810, 43.26054587065083012, 27.80876104995653719 ) ) ;
#4558 = LINE ( 'NONE', #9373, #12763 ) ;
#4559 = ORIENTED_EDGE ( 'NONE', *, *, #6252, .F. ) ;
#4560 = EDGE_CURVE ( 'NONE', #16071, #20875, #13153, .T. ) ;
#4561 = EDGE_CURVE ( 'NONE', #4617, #2915, #19598, .T. ) ;
#4562 = ORIENTED_EDGE ( 'NONE', *, *, #4196, .F. ) ;
#4563 = CIRCLE ( 'NONE', #7082, 0.04999999999999991257 ) ;
#4564 = VECTOR ( 'NONE', #15977, 1000.000000000000000 ) ;
#4565 = CARTESIAN_POINT ( 'NONE',  ( 25.37540678000427263, -68.44634676501046044, 7.500000000000000000 ) ) ;
#4566 = CARTESIAN_POINT ( 'NONE',  ( -23.07496371939382129, -2.433385307706763978, 13.33569868627438559 ) ) ;
#4567 = CYLINDRICAL_SURFACE ( 'NONE', #19520, 0.04999999999999991257 ) ;
#4568 = CARTESIAN_POINT ( 'NONE',  ( 30.79999999999999716, 69.70000000000000284, 0.3000000000000039857 ) ) ;
#4569 = CIRCLE ( 'NONE', #21738, 3.500000000000003109 ) ;
#4570 = LINE ( 'NONE', #9614, #9367 ) ;
#4571 = CYLINDRICAL_SURFACE ( 'NONE', #11028, 0.04999999999999991257 ) ;
#4572 = LINE ( 'NONE', #6048, #7760 ) ;
#4573 = CARTESIAN_POINT ( 'NONE',  ( -30.37540678000427619, 0.000000000000000000, 7.200000000000000178 ) ) ;
#4574 = EDGE_LOOP ( 'NONE', ( #11819, #8054, #1437, #13165 ) ) ;
#4575 = LINE ( 'NONE', #19685, #7366 ) ;
#4576 = EDGE_CURVE ( 'NONE', #16984, #17187, #10314, .T. ) ;
#4577 = CARTESIAN_POINT ( 'NONE',  ( 29.69597781366221767, 27.99124249474150972, 70.25000000000000000 ) ) ;
#4578 = LINE ( 'NONE', #18103, #12214 ) ;
#4579 = AXIS2_PLACEMENT_3D ( 'NONE', #6399, #13199, #4706 ) ;
#4580 = VECTOR ( 'NONE', #16859, 1000.000000000000000 ) ;
#4581 = ORIENTED_EDGE ( 'NONE', *, *, #11069, .F. ) ;
#4582 = CARTESIAN_POINT ( 'NONE',  ( -14.71174975910705029, 51.61873716947361856, 68.25000000000000000 ) ) ;
#4583 = DIRECTION ( 'NONE',  ( 1.000000000000000000, 0.000000000000000000, 6.938893903907222067E-15 ) ) ;
#4584 = ORIENTED_EDGE ( 'NONE', *, *, #2567, .T. ) ;
#4585 = AXIS2_PLACEMENT_3D ( 'NONE', #21152, #5600, #10837 ) ;
#4586 = ORIENTED_EDGE ( 'NONE', *, *, #10757, .F. ) ;
#4587 = CIRCLE ( 'NONE', #7455, 1.000000000000000888 ) ;
#4588 = DIRECTION ( 'NONE',  ( 0.000000000000000000, 0.000000000000000000, -1.000000000000000000 ) ) ;
#4589 = CIRCLE ( 'NONE', #19237, 6.499999999999999112 ) ;
#4590 = EDGE_CURVE ( 'NONE', #2243, #1947, #12246, .T. ) ;
#4591 = EDGE_CURVE ( 'NONE', #10531, #12330, #3666, .T. ) ;
#4592 = EDGE_CURVE ( 'NONE', #6442, #2469, #5016, .T. ) ;
#4593 = ORIENTED_EDGE ( 'NONE', *, *, #11664, .T. ) ;
#4594 = EDGE_CURVE ( 'NONE', #8084, #11165, #17294, .T. ) ;
#4595 = CYLINDRICAL_SURFACE ( 'NONE', #21173, 0.5000000000000004441 ) ;
#4596 = DIRECTION ( 'NONE',  ( -1.224646799147353207E-16, -0.000000000000000000, -1.000000000000000000 ) ) ;
#4597 = AXIS2_PLACEMENT_3D ( 'NONE', #17053, #20534, #6901 ) ;
#4598 = CIRCLE ( 'NONE', #11378, 0.04999999999999991257 ) ;
#4599 = DIRECTION ( 'NONE',  ( -1.000000000000000000, 0.000000000000000000, 0.000000000000000000 ) ) ;
#4600 = DIRECTION ( 'NONE',  ( 0.000000000000000000, 1.000000000000000000, 0.000000000000000000 ) ) ;
#4601 = FACE_OUTER_BOUND ( 'NONE', #17462, .T. ) ;
#4602 = TOROIDAL_SURFACE ( 'NONE', #13879, 0.05000000000000000278, 0.05000000000000000278 ) ;
#4603 = AXIS2_PLACEMENT_3D ( 'NONE', #2261, #7210, #20750 ) ;
#4604 = CARTESIAN_POINT ( 'NONE',  ( 0.000000000000000000, -66.94634676501046044, 13.19999999999999929 ) ) ;
#4605 = CIRCLE ( 'NONE', #19596, 0.2999999999999999334 ) ;
#4606 = DIRECTION ( 'NONE',  ( 0.000000000000000000, 1.000000000000000000, 0.000000000000000000 ) ) ;
#4607 = TOROIDAL_SURFACE ( 'NONE', #1028, 0.7000000000000000666, 0.2999999999999999889 ) ;
#4608 = ADVANCED_FACE ( 'NONE', ( #3331 ), #83, .T. ) ;
#4609 = CARTESIAN_POINT ( 'NONE',  ( -15.95292532278785913, 52.11873716947361856, 14.00000000000000000 ) ) ;
#4610 = DIRECTION ( 'NONE',  ( -1.000000000000000000, 0.000000000000000000, 0.000000000000000000 ) ) ;
#4611 = CYLINDRICAL_SURFACE ( 'NONE', #5551, 0.2999999999999999334 ) ;
#4612 = ORIENTED_EDGE ( 'NONE', *, *, #11921, .T. ) ;
#4613 = ORIENTED_EDGE ( 'NONE', *, *, #10091, .T. ) ;
#4614 = CARTESIAN_POINT ( 'NONE',  ( 15.95292532278785913, -52.11873716947361856, 68.00000000000000000 ) ) ;
#4615 = CIRCLE ( 'NONE', #4965, 0.2999999999999999334 ) ;
#4616 = LINE ( 'NONE', #14665, #9943 ) ;
#4617 = VERTEX_POINT ( 'NONE', #18654 ) ;
#4618 = CARTESIAN_POINT ( 'NONE',  ( 9.641460742840918030, -32.11873716947361856, 109.6002446535588319 ) ) ;
#4619 =( NAMED_UNIT ( * ) SI_UNIT ( $, .STERADIAN. ) SOLID_ANGLE_UNIT ( ) );
#4620 = UNCERTAINTY_MEASURE_WITH_UNIT (LENGTH_MEASURE( 1.000000000000000082E-05 ), #13765, 'distance_accuracy_value', 'NONE');
#4621 = EDGE_CURVE ( 'NONE', #18749, #12515, #288, .T. ) ;
#4622 = LINE ( 'NONE', #19832, #2858 ) ;
#4623 = EDGE_LOOP ( 'NONE', ( #12492, #15536, #18232, #18909 ) ) ;
#4624 = EDGE_CURVE ( 'NONE', #14279, #21390, #10152, .T. ) ;
#4625 = TOROIDAL_SURFACE ( 'NONE', #12821, 1.500000000000000000, 0.5000000000000000000 ) ;
#4626 = ORIENTED_EDGE ( 'NONE', *, *, #19090, .F. ) ;
#4627 = ORIENTED_EDGE ( 'NONE', *, *, #20173, .T. ) ;
#4628 = LINE ( 'NONE', #7648, #2803 ) ;
#4629 = CARTESIAN_POINT ( 'NONE',  ( -1.724728116533986721, 43.26054587065083012, 51.75876104995654003 ) ) ;
#4630 = VERTEX_POINT ( 'NONE', #5357 ) ;
#4631 = CYLINDRICAL_SURFACE ( 'NONE', #8608, 0.5000000000000004441 ) ;
#4632 = DIRECTION ( 'NONE',  ( 0.000000000000000000, 0.000000000000000000, 1.000000000000000000 ) ) ;
#4633 = AXIS2_PLACEMENT_3D ( 'NONE', #4812, #15437, #111 ) ;
#4634 = DIRECTION ( 'NONE',  ( -0.000000000000000000, 0.000000000000000000, -1.000000000000000000 ) ) ;
#4635 = CARTESIAN_POINT ( 'NONE',  ( -27.37540678000428684, -36.74634676501047181, 13.79999999999999893 ) ) ;
#4636 = EDGE_CURVE ( 'NONE', #4677, #11393, #14942, .T. ) ;
#4637 = ORIENTED_EDGE ( 'NONE', *, *, #15199, .F. ) ;
#4638 = LINE ( 'NONE', #9555, #21870 ) ;
#4639 = EDGE_CURVE ( 'NONE', #18412, #7172, #12790, .T. ) ;
#4640 = ORIENTED_EDGE ( 'NONE', *, *, #19813, .T. ) ;
#4641 = EDGE_LOOP ( 'NONE', ( #3577, #10756, #2132 ) ) ;
#4642 = VERTEX_POINT ( 'NONE', #20787 ) ;
#4643 = CARTESIAN_POINT ( 'NONE',  ( -30.19999999999999574, 69.70000000000001705, 0.2999999999999999334 ) ) ;
#4644 = DIRECTION ( 'NONE',  ( -0.000000000000000000, 1.000000000000000000, -0.000000000000000000 ) ) ;
#4645 = ORIENTED_EDGE ( 'NONE', *, *, #15304, .F. ) ;
#4646 = DIRECTION ( 'NONE',  ( -0.000000000000000000, 1.000000000000000000, 0.000000000000000000 ) ) ;
#4647 = EDGE_CURVE ( 'NONE', #15826, #8963, #20686, .T. ) ;
#4648 = CIRCLE ( 'NONE', #8931, 0.1000000000000028644 ) ;
#4649 = CIRCLE ( 'NONE', #11426, 1.250000000000001110 ) ;
#4650 = PRODUCT_DEFINITION_SHAPE ( 'NONE', 'NONE',  #22173 ) ;
#4651 = VERTEX_POINT ( 'NONE', #10270 ) ;
#4652 = CARTESIAN_POINT ( 'NONE',  ( -6.678906393579158163, 42.46645089659918426, 74.06027860057353962 ) ) ;
#4653 = LINE ( 'NONE', #11461, #4170 ) ;
#4654 = DIRECTION ( 'NONE',  ( 0.000000000000000000, 0.000000000000000000, -1.000000000000000000 ) ) ;
#4655 = CYLINDRICAL_SURFACE ( 'NONE', #20583, 0.2999999999999999334 ) ;
#4656 = EDGE_LOOP ( 'NONE', ( #5783, #14027, #6646, #11884 ) ) ;
#4657 = DIRECTION ( 'NONE',  ( 0.000000000000000000, 0.000000000000000000, 1.000000000000000000 ) ) ;
#4658 = DIRECTION ( 'NONE',  ( 0.000000000000000000, 0.000000000000000000, -1.000000000000000000 ) ) ;
#4659 = B_SPLINE_CURVE_WITH_KNOTS ( 'NONE', 3,
 ( #6414, #2926, #11625, #9754, #13210, #16553 ),
 .UNSPECIFIED., .F., .F.,
 ( 4, 2, 4 ),
 ( 0.000000000000000000, 0.0002343433793794306779, 0.0004686867587588613559 ),
 .UNSPECIFIED. ) ;
#4660 = DIRECTION ( 'NONE',  ( 0.000000000000000000, 0.000000000000000000, 1.000000000000000000 ) ) ;
#4661 = CARTESIAN_POINT ( 'NONE',  ( -23.61959064016851073, 45.26242829375641463, 68.25000000000000000 ) ) ;
#4662 = EDGE_LOOP ( 'NONE', ( #16737, #21248, #2462, #1151 ) ) ;
#4663 = LINE ( 'NONE', #8455, #20582 ) ;
#4664 = CARTESIAN_POINT ( 'NONE',  ( -25.37540678000427263, -68.74634676501045760, 7.200000000000000178 ) ) ;
#4665 = AXIS2_PLACEMENT_3D ( 'NONE', #10352, #13249, #4980 ) ;
#4666 = EDGE_CURVE ( 'NONE', #10568, #8021, #17091, .T. ) ;
#4667 = ORIENTED_EDGE ( 'NONE', *, *, #546, .F. ) ;
#4668 = CIRCLE ( 'NONE', #13230, 0.3000000000000016542 ) ;
#4669 = CARTESIAN_POINT ( 'NONE',  ( -27.37540678000426908, 36.74634676501047181, 42.50000000000000000 ) ) ;
#4670 = CARTESIAN_POINT ( 'NONE',  ( -14.96174975910705207, 51.86873716947361856, 68.00000000000000000 ) ) ;
#4671 = EDGE_CURVE ( 'NONE', #16591, #4986, #5325, .T. ) ;
#4672 = ORIENTED_EDGE ( 'NONE', *, *, #12542, .F. ) ;
#4673 = VERTEX_POINT ( 'NONE', #13712 ) ;
#4674 = VERTEX_POINT ( 'NONE', #12034 ) ;
#4675 = LINE ( 'NONE', #18409, #6715 ) ;
#4676 = CARTESIAN_POINT ( 'NONE',  ( 26.37540678000427619, 10.94079601157914539, 42.50000000000000000 ) ) ;
#4677 = VERTEX_POINT ( 'NONE', #8601 ) ;
#4678 = VERTEX_POINT ( 'NONE', #22025 ) ;
#4679 = CARTESIAN_POINT ( 'NONE',  ( -1.724728116533986721, 43.26054587065083012, 39.80876104995653719 ) ) ;
#4680 = CIRCLE ( 'NONE', #15034, 0.05000000000000143219 ) ;
#4681 = LINE ( 'NONE', #1299, #11333 ) ;
#4682 = CARTESIAN_POINT ( 'NONE',  ( -23.04884263981454140, -2.295195349811812946, 13.26498523032724997 ) ) ;
#4683 = VECTOR ( 'NONE', #20049, 1000.000000000000000 ) ;
#4684 = FACE_OUTER_BOUND ( 'NONE', #20476, .T. ) ;
#4685 = EDGE_CURVE ( 'NONE', #14491, #18912, #6745, .T. ) ;
#4686 = DIRECTION ( 'NONE',  ( 1.000000000000000000, 0.000000000000000000, 0.000000000000000000 ) ) ;
#4687 = DIRECTION ( 'NONE',  ( 1.000000000000000000, 0.000000000000000000, 0.000000000000000000 ) ) ;
#4688 = ORIENTED_EDGE ( 'NONE', *, *, #2729, .F. ) ;
#4689 = CARTESIAN_POINT ( 'NONE',  ( -29.50000000000002132, 0.000000000000000000, 0.2999999999999947153 ) ) ;
#4690 = CARTESIAN_POINT ( 'NONE',  ( 9.641460742840918030, -32.61873716947361856, 68.00000000000000000 ) ) ;
#4691 = CARTESIAN_POINT ( 'NONE',  ( 1.824728116533979705, 43.26054587065083012, 41.66679706732590915 ) ) ;
#4692 = VERTEX_POINT ( 'NONE', #6701 ) ;
#4693 = CARTESIAN_POINT ( 'NONE',  ( 1.774728116533979438, 42.36054587065083155, 39.80876104995653719 ) ) ;
#4694 = EDGE_CURVE ( 'NONE', #22137, #4942, #17800, .T. ) ;
#4695 = CARTESIAN_POINT ( 'NONE',  ( -24.43662752439705343, 0.000000000000000000, 3.500000000000000000 ) ) ;
#4696 = ORIENTED_EDGE ( 'NONE', *, *, #2918, .F. ) ;
#4697 = CARTESIAN_POINT ( 'NONE',  ( -1.724728116533986721, 43.31054587065082728, 35.80876104995653009 ) ) ;
#4698 = VECTOR ( 'NONE', #3328, 1000.000000000000000 ) ;
#4699 = ORIENTED_EDGE ( 'NONE', *, *, #13018, .T. ) ;
#4700 = ORIENTED_EDGE ( 'NONE', *, *, #20532, .F. ) ;
#4701 = CARTESIAN_POINT ( 'NONE',  ( -8.641460742840918030, -33.93424481021354921, 68.50000000000000000 ) ) ;
#4702 = AXIS2_PLACEMENT_3D ( 'NONE', #14022, #4180, #13913 ) ;
#4703 = EDGE_LOOP ( 'NONE', ( #19111, #18557, #15737, #10475 ) ) ;
#4704 = VECTOR ( 'NONE', #18184, 1000.000000000000000 ) ;
#4705 = EDGE_CURVE ( 'NONE', #17039, #11890, #4589, .T. ) ;
#4706 = DIRECTION ( 'NONE',  ( 2.107255972849994642E-16, 0.000000000000000000, 1.000000000000000000 ) ) ;
#4707 = DIRECTION ( 'NONE',  ( 0.000000000000000000, 0.000000000000000000, 1.000000000000000000 ) ) ;
#4708 = VECTOR ( 'NONE', #13237, 1000.000000000000000 ) ;
#4709 =( BOUNDED_CURVE ( )  B_SPLINE_CURVE ( 3, ( #8149, #9477, #4784, #2892 ),
 .UNSPECIFIED., .F., .T. ) 
 B_SPLINE_CURVE_WITH_KNOTS ( ( 4, 4 ),
 ( 1.570796326794896558, 3.141592653589793116 ),
 .UNSPECIFIED. ) 
 CURVE ( )  GEOMETRIC_REPRESENTATION_ITEM ( )  RATIONAL_B_SPLINE_CURVE ( ( 1.000000000000000000, 0.8047378541243649375, 0.8047378541243649375, 1.000000000000000000 ) ) 
 REPRESENTATION_ITEM ( '' )  );
#4710 = DIRECTION ( 'NONE',  ( 2.832483164223434527E-16, -1.000000000000000000, 0.000000000000000000 ) ) ;
#4711 = LINE ( 'NONE', #13416, #2364 ) ;
#4712 = CARTESIAN_POINT ( 'NONE',  ( 15.95292532278785913, -52.11873716947361856, 109.6002446535588319 ) ) ;
#4713 = FACE_OUTER_BOUND ( 'NONE', #10592, .T. ) ;
#4714 = ADVANCED_FACE ( 'NONE', ( #14373 ), #22108, .T. ) ;
#4715 = CARTESIAN_POINT ( 'NONE',  ( -17.45292532278785913, 34.11873716947361856, 68.00000000000000000 ) ) ;
#4716 = EDGE_CURVE ( 'NONE', #13159, #2540, #13511, .T. ) ;
#4717 = FACE_OUTER_BOUND ( 'NONE', #12537, .T. ) ;
#4718 = DIRECTION ( 'NONE',  ( 0.9729678061520339316, 0.2309407893632007824, 0.000000000000000000 ) ) ;
#4719 = AXIS2_PLACEMENT_3D ( 'NONE', #7249, #20563, #5240 ) ;
#4720 = ORIENTED_EDGE ( 'NONE', *, *, #21987, .F. ) ;
#4721 = AXIS2_PLACEMENT_3D ( 'NONE', #17353, #17681, #2253 ) ;
#4722 = CARTESIAN_POINT ( 'NONE',  ( -1.724728116533986721, 43.26054587065083012, 41.66679706732590915 ) ) ;
#4723 = EDGE_LOOP ( 'NONE', ( #16532, #9709, #19344, #10484 ) ) ;
#4724 = DIRECTION ( 'NONE',  ( -0.000000000000000000, 0.000000000000000000, 1.000000000000000000 ) ) ;
#4725 = AXIS2_PLACEMENT_3D ( 'NONE', #20837, #18936, #548 ) ;
#4726 = VECTOR ( 'NONE', #7895, 1000.000000000000000 ) ;
#4727 = DIRECTION ( 'NONE',  ( 1.000000000000000000, 0.000000000000000000, 0.000000000000000000 ) ) ;
#4728 = VERTEX_POINT ( 'NONE', #14150 ) ;
#4729 = ORIENTED_EDGE ( 'NONE', *, *, #13448, .F. ) ;
#4730 = CARTESIAN_POINT ( 'NONE',  ( 8.641460742840918030, 33.43424481021354921, 68.00000000000000000 ) ) ;
#4731 =( NAMED_UNIT ( * ) PLANE_ANGLE_UNIT ( ) SI_UNIT ( $, .RADIAN. ) );
#4732 = ORIENTED_EDGE ( 'NONE', *, *, #10041, .T. ) ;
#4733 = EDGE_LOOP ( 'NONE', ( #16963, #8147, #1884, #6727 ) ) ;
#4734 = EDGE_CURVE ( 'NONE', #17367, #14785, #15638, .T. ) ;
#4735 = EDGE_LOOP ( 'NONE', ( #11557, #6819, #20901, #8235 ) ) ;
#4736 = ORIENTED_EDGE ( 'NONE', *, *, #10052, .T. ) ;
#4737 = VECTOR ( 'NONE', #7281, 1000.000000000000000 ) ;
#4738 = DIRECTION ( 'NONE',  ( 0.000000000000000000, 0.000000000000000000, 1.000000000000000000 ) ) ;
#4739 = AXIS2_PLACEMENT_3D ( 'NONE', #10303, #1791, #13736 ) ;
#4740 = DIRECTION ( 'NONE',  ( 0.000000000000000000, -0.000000000000000000, 1.000000000000000000 ) ) ;
#4741 = EDGE_LOOP ( 'NONE', ( #15216, #13158, #10326, #22068 ) ) ;
#4742 = CARTESIAN_POINT ( 'NONE',  ( -23.32398829872514057, 3.528912754968630328, 13.50000000000000000 ) ) ;
#4743 = EDGE_CURVE ( 'NONE', #3965, #412, #9961, .T. ) ;
#4744 = CARTESIAN_POINT ( 'NONE',  ( -15.95292532278785913, -50.11873716947361856, 13.50000000000000000 ) ) ;
#4745 = EDGE_CURVE ( 'NONE', #14293, #8250, #18504, .T. ) ;
#4746 = CARTESIAN_POINT ( 'NONE',  ( 28.57540678000427548, -6.494748934539263274, 13.50000000000000000 ) ) ;
#4747 = FACE_OUTER_BOUND ( 'NONE', #21178, .T. ) ;
#4748 = CIRCLE ( 'NONE', #6553, 0.5000000000000004441 ) ;
#4749 = ADVANCED_FACE ( 'NONE', ( #21001 ), #2194, .T. ) ;
#4750 = CARTESIAN_POINT ( 'NONE',  ( -21.92816239687475743, 42.46645089659918426, 13.74999999999999822 ) ) ;
#4751 = ORIENTED_EDGE ( 'NONE', *, *, #18376, .F. ) ;
#4752 = ORIENTED_EDGE ( 'NONE', *, *, #3606, .T. ) ;
#4753 = ORIENTED_EDGE ( 'NONE', *, *, #9935, .F. ) ;
#4754 = CARTESIAN_POINT ( 'NONE',  ( 17.95292532278785913, 50.11873716947361856, 109.6002446535588319 ) ) ;
#4755 = DIRECTION ( 'NONE',  ( 0.000000000000000000, 0.000000000000000000, 1.000000000000000000 ) ) ;
#4756 = EDGE_LOOP ( 'NONE', ( #7377, #21979, #9379, #3777, #5288, #14281 ) ) ;
#4757 = DIRECTION ( 'NONE',  ( 0.000000000000000000, 0.000000000000000000, 1.000000000000000000 ) ) ;
#4758 = EDGE_CURVE ( 'NONE', #20751, #2319, #2799, .T. ) ;
#4759 = ORIENTED_EDGE ( 'NONE', *, *, #12873, .T. ) ;
#4760 = CARTESIAN_POINT ( 'NONE',  ( -1.724728116533986721, 42.36054587065083155, 49.66679706732590915 ) ) ;
#4761 = CARTESIAN_POINT ( 'NONE',  ( 29.69597781366221767, 27.99124249474150972, 70.50000000000000000 ) ) ;
#4762 = EDGE_CURVE ( 'NONE', #15775, #21768, #10911, .T. ) ;
#4763 = CARTESIAN_POINT ( 'NONE',  ( 0.000000000000000000, -71.70000000000001705, 1.500000000000000000 ) ) ;
#4764 = CARTESIAN_POINT ( 'NONE',  ( 31.44597781366222122, 27.99124249474150972, 68.50000000000000000 ) ) ;
#4765 = EDGE_LOOP ( 'NONE', ( #16034, #11762, #18041 ) ) ;
#4766 = CARTESIAN_POINT ( 'NONE',  ( -8.641460742840918030, 32.93424481021354921, 7.321391277662001151 ) ) ;
#4767 = CARTESIAN_POINT ( 'NONE',  ( -24.13662752439704917, 0.000000000000000000, 7.500000000000000000 ) ) ;
#4768 = CARTESIAN_POINT ( 'NONE',  ( -34.70000000000000284, -85.00000000000000000, 0.6000000000000033085 ) ) ;
#4769 = CARTESIAN_POINT ( 'NONE',  ( -20.53081511603577169, 86.49759185912192549, 68.25000000000000000 ) ) ;
#4770 = ORIENTED_EDGE ( 'NONE', *, *, #21113, .F. ) ;
#4771 = FACE_OUTER_BOUND ( 'NONE', #7356, .T. ) ;
#4772 = EDGE_CURVE ( 'NONE', #17156, #3943, #15303, .T. ) ;
#4773 = VERTEX_POINT ( 'NONE', #12675 ) ;
#4774 = FACE_OUTER_BOUND ( 'NONE', #2766, .T. ) ;
#4775 = CARTESIAN_POINT ( 'NONE',  ( -26.33662752439704846, 0.000000000000000000, 0.3000000000000016542 ) ) ;
#4776 = EDGE_LOOP ( 'NONE', ( #15723, #20634, #16976, #536 ) ) ;
#4777 = ORIENTED_EDGE ( 'NONE', *, *, #17161, .T. ) ;
#4778 = ORIENTED_EDGE ( 'NONE', *, *, #2699, .F. ) ;
#4779 = CARTESIAN_POINT ( 'NONE',  ( -33.80000000000001847, 84.70000000000001705, 78.20000000000000284 ) ) ;
#4780 = CARTESIAN_POINT ( 'NONE',  ( 17.95292532278785913, -38.74634676501045760, 14.00000000000000000 ) ) ;
#4781 = ORIENTED_EDGE ( 'NONE', *, *, #5605, .T. ) ;
#4782 = CARTESIAN_POINT ( 'NONE',  ( -1.724728116533986721, 43.26054587065083012, 51.80876104995653719 ) ) ;
#4783 = ORIENTED_EDGE ( 'NONE', *, *, #17568, .T. ) ;
#4784 = CARTESIAN_POINT ( 'NONE',  ( 29.50000000000001421, 69.00000000000000000, 0.1242640687119232062 ) ) ;
#4785 = EDGE_CURVE ( 'NONE', #21235, #3651, #12580, .T. ) ;
#4786 = CARTESIAN_POINT ( 'NONE',  ( -29.13662752439705272, 0.000000000000000000, 0.000000000000000000 ) ) ;
#4787 = CARTESIAN_POINT ( 'NONE',  ( -23.18291235612340273, -2.947575143997166247, 13.45754841673216085 ) ) ;
#4788 = CARTESIAN_POINT ( 'NONE',  ( -1.824728116533986810, 43.26054587065083012, 47.80876104995653719 ) ) ;
#4789 = ADVANCED_FACE ( 'NONE', ( #3999 ), #615, .F. ) ;
#4790 = CARTESIAN_POINT ( 'NONE',  ( -1.724728116533986721, 43.31054587065082728, 39.70876104995653577 ) ) ;
#4791 = CARTESIAN_POINT ( 'NONE',  ( 0.000000000000000000, 43.26054587065083012, 43.75876104995654003 ) ) ;
#4792 = EDGE_LOOP ( 'NONE', ( #12574, #17888, #8310, #13332 ) ) ;
#4793 = DIRECTION ( 'NONE',  ( -1.000000000000000000, 0.000000000000000000, 0.000000000000000000 ) ) ;
#4794 = CYLINDRICAL_SURFACE ( 'NONE', #17396, 0.05000000000000143219 ) ;
#4795 = DIRECTION ( 'NONE',  ( 1.000000000000000000, 0.000000000000000000, 0.000000000000000000 ) ) ;
#4796 = FACE_OUTER_BOUND ( 'NONE', #9758, .T. ) ;
#4797 = ORIENTED_EDGE ( 'NONE', *, *, #21691, .T. ) ;
#4798 = DIRECTION ( 'NONE',  ( 4.336808689941893885E-15, 0.000000000000000000, 1.000000000000000000 ) ) ;
#4799 = VERTEX_POINT ( 'NONE', #12470 ) ;
#4800 = CARTESIAN_POINT ( 'NONE',  ( 9.178906393579156386, 42.46645089659917716, 69.50000000000000000 ) ) ;
#4801 = ORIENTED_EDGE ( 'NONE', *, *, #13708, .F. ) ;
#4802 = EDGE_CURVE ( 'NONE', #5916, #1488, #9244, .T. ) ;
#4803 = ADVANCED_FACE ( 'NONE', ( #14045 ), #16047, .F. ) ;
#4804 = EDGE_LOOP ( 'NONE', ( #5009, #1772, #2418, #17777 ) ) ;
#4805 = CYLINDRICAL_SURFACE ( 'NONE', #20985, 0.5000000000000004441 ) ;
#4806 = EDGE_LOOP ( 'NONE', ( #3823, #7052, #46, #7973 ) ) ;
#4807 = EDGE_CURVE ( 'NONE', #8747, #19185, #4204, .T. ) ;
#4808 = CARTESIAN_POINT ( 'NONE',  ( -1.824728116533986810, 42.36054587065083155, 51.70876104995653577 ) ) ;
#4809 = CARTESIAN_POINT ( 'NONE',  ( 3.627054932750481964, -32.93424481021354921, 68.50000000000000000 ) ) ;
#4810 = DIRECTION ( 'NONE',  ( 0.000000000000000000, 0.000000000000000000, -1.000000000000000000 ) ) ;
#4811 = DIRECTION ( 'NONE',  ( 0.000000000000000000, -1.000000000000000000, 0.000000000000000000 ) ) ;
#4812 = CARTESIAN_POINT ( 'NONE',  ( -32.20000000000001705, 71.00000000000001421, 1.800000000000000044 ) ) ;
#4813 = CARTESIAN_POINT ( 'NONE',  ( -29.13662752439705272, 0.000000000000000000, 13.19999999999999929 ) ) ;
#4814 = DIRECTION ( 'NONE',  ( 0.000000000000000000, 0.000000000000000000, 1.000000000000000000 ) ) ;
#4815 = DIRECTION ( 'NONE',  ( 2.388292521039847891E-16, -0.000000000000000000, 1.000000000000000000 ) ) ;
#4816 = FACE_OUTER_BOUND ( 'NONE', #10267, .T. ) ;
#4817 = AXIS2_PLACEMENT_3D ( 'NONE', #17420, #2313, #631 ) ;
#4818 = TOROIDAL_SURFACE ( 'NONE', #9826, 0.05000000000000000278, 0.05000000000000000278 ) ;
#4819 = ADVANCED_FACE ( 'NONE', ( #16155 ), #19648, .T. ) ;
#4820 = VERTEX_POINT ( 'NONE', #11130 ) ;
#4821 = DIRECTION ( 'NONE',  ( 1.000000000000000000, 0.000000000000000000, 0.000000000000000000 ) ) ;
#4822 = EDGE_LOOP ( 'NONE', ( #6918, #1515, #7430, #16958 ) ) ;
#4823 = CARTESIAN_POINT ( 'NONE',  ( -27.67540678000426979, 36.74634676501047181, 13.50000000000000000 ) ) ;
#4824 = CARTESIAN_POINT ( 'NONE',  ( 1.724728116533979616, 43.31054587065082728, 31.75876104995653648 ) ) ;
#4825 = ORIENTED_EDGE ( 'NONE', *, *, #16153, .T. ) ;
#4826 = ORIENTED_EDGE ( 'NONE', *, *, #1093, .T. ) ;
#4827 = DIRECTION ( 'NONE',  ( 0.000000000000000000, 0.000000000000000000, 1.000000000000000000 ) ) ;
#4828 = CARTESIAN_POINT ( 'NONE',  ( 0.000000000000000000, 0.000000000000000000, 0.000000000000000000 ) ) ;
#4829 = ORIENTED_EDGE ( 'NONE', *, *, #7348, .F. ) ;
#4830 = LINE ( 'NONE', #16567, #3213 ) ;
#4831 = ORIENTED_EDGE ( 'NONE', *, *, #10604, .T. ) ;
#4832 = EDGE_CURVE ( 'NONE', #7436, #16130, #11634, .T. ) ;
#4833 = ORIENTED_EDGE ( 'NONE', *, *, #14040, .F. ) ;
#4834 = EDGE_CURVE ( 'NONE', #19467, #9554, #7381, .T. ) ;
#4835 = TOROIDAL_SURFACE ( 'NONE', #9127, 2.767785046117003489, 0.2500000000000000000 ) ;
#4836 = VECTOR ( 'NONE', #15837, 1000.000000000000000 ) ;
#4837 = ORIENTED_EDGE ( 'NONE', *, *, #13134, .T. ) ;
#4838 = LINE ( 'NONE', #9993, #3124 ) ;
#4839 = LINE ( 'NONE', #3280, #10663 ) ;
#4840 = ORIENTED_EDGE ( 'NONE', *, *, #19475, .T. ) ;
#4841 = CARTESIAN_POINT ( 'NONE',  ( -23.49018890325625364, 45.04852366434393218, 68.25000000000000000 ) ) ;
#4842 = CARTESIAN_POINT ( 'NONE',  ( -23.02398829872514341, 2.928406208502772667, 13.54172988673450639 ) ) ;
#4843 = PLANE ( 'NONE',  #74 ) ;
#4844 = FACE_OUTER_BOUND ( 'NONE', #523, .T. ) ;
#4845 = TOROIDAL_SURFACE ( 'NONE', #9491, 0.05000000000000000278, 0.05000000000000000278 ) ;
#4846 = EDGE_CURVE ( 'NONE', #961, #1826, #7793, .T. ) ;
#4847 = DIRECTION ( 'NONE',  ( 0.000000000000000000, -0.000000000000000000, -1.000000000000000000 ) ) ;
#4848 = ORIENTED_EDGE ( 'NONE', *, *, #5728, .F. ) ;
#4849 = TOROIDAL_SURFACE ( 'NONE', #7732, 0.2500000000000000000, 0.2500000000000000000 ) ;
#4850 = ORIENTED_EDGE ( 'NONE', *, *, #3471, .F. ) ;
#4851 = CIRCLE ( 'NONE', #19489, 4.051418481279135619 ) ;
#4852 = VECTOR ( 'NONE', #19993, 1000.000000000000000 ) ;
#4853 = ORIENTED_EDGE ( 'NONE', *, *, #13334, .T. ) ;
#4854 = DIRECTION ( 'NONE',  ( -1.000000000000000000, 0.000000000000000000, -6.123233995736764803E-17 ) ) ;
#4855 = PLANE ( 'NONE',  #19928 ) ;
#4856 = VERTEX_POINT ( 'NONE', #7907 ) ;
#4857 = DIRECTION ( 'NONE',  ( -1.000000000000000000, 0.000000000000000000, 0.000000000000000000 ) ) ;
#4858 = EDGE_CURVE ( 'NONE', #15168, #14169, #912, .T. ) ;
#4859 = ADVANCED_FACE ( 'NONE', ( #12912 ), #18434, .F. ) ;
#4860 = VERTEX_POINT ( 'NONE', #11979 ) ;
#4861 = DIRECTION ( 'NONE',  ( 0.000000000000000000, 0.000000000000000000, 1.000000000000000000 ) ) ;
#4862 = CIRCLE ( 'NONE', #18448, 0.05000000000000143219 ) ;
#4863 = VECTOR ( 'NONE', #1315, 1000.000000000000000 ) ;
#4864 = AXIS2_PLACEMENT_3D ( 'NONE', #4268, #16323, #19704 ) ;
#4865 = DIRECTION ( 'NONE',  ( 1.000000000000000000, -0.000000000000000000, -0.000000000000000000 ) ) ;
#4866 = EDGE_CURVE ( 'NONE', #6508, #14913, #19160, .T. ) ;
#4867 = DIRECTION ( 'NONE',  ( 1.000000000000000000, 0.000000000000000000, 0.000000000000000000 ) ) ;
#4868 = VECTOR ( 'NONE', #17578, 1000.000000000000000 ) ;
#4869 = CARTESIAN_POINT ( 'NONE',  ( -31.50000000000002132, 71.70000000000001705, 3.200000000000000178 ) ) ;
#4870 = VECTOR ( 'NONE', #17054, 1000.000000000000000 ) ;
#4871 = ORIENTED_EDGE ( 'NONE', *, *, #319, .T. ) ;
#4872 = DIRECTION ( 'NONE',  ( -1.000000000000000000, 0.000000000000000000, 0.000000000000000000 ) ) ;
#4873 = CARTESIAN_POINT ( 'NONE',  ( -1.824728116533986810, 43.26054587065083012, 51.80876104995653719 ) ) ;
#4874 = LINE ( 'NONE', #20865, #4349 ) ;
#4875 = CYLINDRICAL_SURFACE ( 'NONE', #17651, 0.04999999999999991257 ) ;
#4876 = DIRECTION ( 'NONE',  ( 1.224646799147353207E-16, 0.000000000000000000, 1.000000000000000000 ) ) ;
#4877 = ORIENTED_EDGE ( 'NONE', *, *, #15400, .T. ) ;
#4878 = DIRECTION ( 'NONE',  ( 0.000000000000000000, 0.000000000000000000, 1.000000000000000000 ) ) ;
#4879 = EDGE_CURVE ( 'NONE', #857, #9580, #8083, .T. ) ;
#4880 = ORIENTED_EDGE ( 'NONE', *, *, #14008, .F. ) ;
#4881 = DIRECTION ( 'NONE',  ( 0.000000000000000000, 0.000000000000000000, -1.000000000000000000 ) ) ;
#4882 = DIRECTION ( 'NONE',  ( 0.000000000000000000, 0.000000000000000000, 1.000000000000000000 ) ) ;
#4883 = ORIENTED_EDGE ( 'NONE', *, *, #19816, .F. ) ;
#4884 = EDGE_LOOP ( 'NONE', ( #9073, #1695, #9405, #11477 ) ) ;
#4885 = VECTOR ( 'NONE', #16994, 1000.000000000000227 ) ;
#4886 = ORIENTED_EDGE ( 'NONE', *, *, #11565, .T. ) ;
#4887 = DIRECTION ( 'NONE',  ( 1.000000000000000000, 0.000000000000000000, 0.000000000000000000 ) ) ;
#4888 = DIRECTION ( 'NONE',  ( -6.123233995736764803E-17, 0.000000000000000000, 1.000000000000000000 ) ) ;
#4889 = ORIENTED_EDGE ( 'NONE', *, *, #14414, .F. ) ;
#4890 = CARTESIAN_POINT ( 'NONE',  ( 1.824728116533979261, 43.31054587065082728, 27.70876104995653577 ) ) ;
#4891 = ORIENTED_EDGE ( 'NONE', *, *, #6795, .F. ) ;
#4892 = EDGE_CURVE ( 'NONE', #1527, #12093, #14597, .T. ) ;
#4893 = VERTEX_POINT ( 'NONE', #4957 ) ;
#4894 = CARTESIAN_POINT ( 'NONE',  ( 29.37540678000427619, -4.700000000000000178, 3.500000000000000000 ) ) ;
#4895 = EDGE_CURVE ( 'NONE', #14054, #10473, #6642, .T. ) ;
#4896 = DIRECTION ( 'NONE',  ( 0.000000000000000000, 0.000000000000000000, 1.000000000000000000 ) ) ;
#4897 = CARTESIAN_POINT ( 'NONE',  ( -23.02398829872490538, -3.297879325580993726, 13.54382403646240007 ) ) ;
#4898 = DIRECTION ( 'NONE',  ( 0.000000000000000000, 0.000000000000000000, 1.000000000000000000 ) ) ;
#4899 = CIRCLE ( 'NONE', #8830, 0.5000000000000004441 ) ;
#4900 = AXIS2_PLACEMENT_3D ( 'NONE', #21616, #18568, #13075 ) ;
#4901 = CIRCLE ( 'NONE', #7413, 0.1000000000000028644 ) ;
#4902 = DIRECTION ( 'NONE',  ( 0.000000000000000000, 0.000000000000000000, 1.000000000000000000 ) ) ;
#4903 = CARTESIAN_POINT ( 'NONE',  ( -9.178906393579156386, 42.46645089659917716, 69.50000000000000000 ) ) ;
#4904 = FACE_OUTER_BOUND ( 'NONE', #3219, .T. ) ;
#4905 = VECTOR ( 'NONE', #17878, 1000.000000000000000 ) ;
#4906 = CARTESIAN_POINT ( 'NONE',  ( 0.000000000000000000, -5.000000000000000000, 7.200000000000000178 ) ) ;
#4907 = CARTESIAN_POINT ( 'NONE',  ( -14.96174975910705207, 51.61873716947361856, 68.25000000000000000 ) ) ;
#4908 = ORIENTED_EDGE ( 'NONE', *, *, #20453, .F. ) ;
#4909 = FACE_OUTER_BOUND ( 'NONE', #18635, .T. ) ;
#4910 = AXIS2_PLACEMENT_3D ( 'NONE', #8466, #15494, #10259 ) ;
#4911 = LINE ( 'NONE', #8274, #7380 ) ;
#4912 = VERTEX_POINT ( 'NONE', #3168 ) ;
#4913 = ADVANCED_FACE ( 'NONE', ( #8542 ), #9574, .T. ) ;
#4914 = DIRECTION ( 'NONE',  ( -0.000000000000000000, -0.000000000000000000, -1.000000000000000000 ) ) ;
#4915 = ORIENTED_EDGE ( 'NONE', *, *, #14838, .F. ) ;
#4916 = CIRCLE ( 'NONE', #11682, 0.6000000000000033085 ) ;
#4917 = ADVANCED_FACE ( 'NONE', ( #21563 ), #5231, .T. ) ;
#4918 = AXIS2_PLACEMENT_3D ( 'NONE', #7028, #1866, #8475 ) ;
#4919 = CIRCLE ( 'NONE', #4191, 0.09999999999999939493 ) ;
#4920 = ORIENTED_EDGE ( 'NONE', *, *, #4560, .F. ) ;
#4921 = AXIS2_PLACEMENT_3D ( 'NONE', #1953, #8798, #14039 ) ;
#4922 = AXIS2_PLACEMENT_3D ( 'NONE', #16379, #4305, #14462 ) ;
#4923 = AXIS2_PLACEMENT_3D ( 'NONE', #7975, #19825, #8200 ) ;
#4924 = DIRECTION ( 'NONE',  ( 0.000000000000000000, 0.000000000000000000, -1.000000000000000000 ) ) ;
#4925 = EDGE_LOOP ( 'NONE', ( #5572, #519, #20457, #2439 ) ) ;
#4926 = B_SPLINE_CURVE_WITH_KNOTS ( 'NONE', 3,
 ( #8728, #8508, #8387, #22053, #11845, #13734, #3689, #15526 ),
 .UNSPECIFIED., .F., .F.,
 ( 4, 2, 2, 4 ),
 ( -3.464559252384133923E-06, 0.0002895415592466213275, 0.0004360446184961240686, 0.0005825476777456268639 ),
 .UNSPECIFIED. ) ;
#4927 = CARTESIAN_POINT ( 'NONE',  ( -8.641460742840918030, -32.93424481021354921, 42.50000000000000000 ) ) ;
#4928 = CARTESIAN_POINT ( 'NONE',  ( -31.26086011588028057, 83.95073979834610611, 13.75000000000000000 ) ) ;
#4929 = VECTOR ( 'NONE', #9846, 1000.000000000000000 ) ;
#4930 = CIRCLE ( 'NONE', #4918, 0.5000000000000004441 ) ;
#4931 = VECTOR ( 'NONE', #20698, 1000.000000000000000 ) ;
#4932 = FACE_OUTER_BOUND ( 'NONE', #4081, .T. ) ;
#4933 = CARTESIAN_POINT ( 'NONE',  ( -9.141460742840918030, -32.61873716947361856, 68.50000000000000000 ) ) ;
#4934 = DIRECTION ( 'NONE',  ( -4.078297354714382145E-17, -0.4461977533474358326, -0.8949343913984425525 ) ) ;
#4935 = VECTOR ( 'NONE', #2222, 1000.000000000000000 ) ;
#4936 = CARTESIAN_POINT ( 'NONE',  ( -15.13992500838820909, -52.10286008548567338, 13.87499999123205363 ) ) ;
#4937 = CARTESIAN_POINT ( 'NONE',  ( 33.49999999999998579, 84.70000000000001705, 78.20000000000000284 ) ) ;
#4938 = TOROIDAL_SURFACE ( 'NONE', #2442, 2.299999999999993161, 0.2999999999999999889 ) ;
#4939 = VECTOR ( 'NONE', #9349, 1000.000000000000000 ) ;
#4940 = ORIENTED_EDGE ( 'NONE', *, *, #7389, .F. ) ;
#4941 = DIRECTION ( 'NONE',  ( 0.000000000000000000, 0.000000000000000000, 1.000000000000000000 ) ) ;
#4942 = VERTEX_POINT ( 'NONE', #20509 ) ;
#4943 = DIRECTION ( 'NONE',  ( 0.000000000000000000, -1.000000000000000000, 0.000000000000000000 ) ) ;
#4944 = EDGE_CURVE ( 'NONE', #21163, #17770, #9992, .T. ) ;
#4945 = DIRECTION ( 'NONE',  ( -1.000000000000000000, 0.000000000000000000, 0.000000000000000000 ) ) ;
#4946 = ORIENTED_EDGE ( 'NONE', *, *, #20132, .F. ) ;
#4947 = VERTEX_POINT ( 'NONE', #4532 ) ;
#4948 = DIRECTION ( 'NONE',  ( -2.107255972849994642E-16, 0.000000000000000000, -1.000000000000000000 ) ) ;
#4949 = ORIENTED_EDGE ( 'NONE', *, *, #1405, .T. ) ;
#4950 = AXIS2_PLACEMENT_3D ( 'NONE', #6699, #5015, #11814 ) ;
#4951 = AXIS2_PLACEMENT_3D ( 'NONE', #17142, #3499, #20511 ) ;
#4952 = ORIENTED_EDGE ( 'NONE', *, *, #10479, .T. ) ;
#4953 = VECTOR ( 'NONE', #13286, 1000.000000000000000 ) ;
#4954 = AXIS2_PLACEMENT_3D ( 'NONE', #5939, #9630, #4364 ) ;
#4955 = ORIENTED_EDGE ( 'NONE', *, *, #3300, .F. ) ;
#4956 = TOROIDAL_SURFACE ( 'NONE', #7477, 2.274596669241483848, 0.2999999999999999889 ) ;
#4957 = CARTESIAN_POINT ( 'NONE',  ( 30.37540678000427619, -63.74634676501045050, 3.799999999999999822 ) ) ;
#4958 = LINE ( 'NONE', #20403, #10325 ) ;
#4959 = EDGE_CURVE ( 'NONE', #16140, #15183, #4504, .T. ) ;
#4960 = FACE_OUTER_BOUND ( 'NONE', #13007, .T. ) ;
#4961 = ORIENTED_EDGE ( 'NONE', *, *, #18483, .F. ) ;
#4962 = DIRECTION ( 'NONE',  ( 0.000000000000000000, 0.000000000000000000, 1.000000000000000000 ) ) ;
#4963 = DIRECTION ( 'NONE',  ( 0.000000000000000000, 1.000000000000000000, 0.000000000000000000 ) ) ;
#4964 = DIRECTION ( 'NONE',  ( 0.000000000000000000, 0.000000000000000000, 1.000000000000000000 ) ) ;
#4965 = AXIS2_PLACEMENT_3D ( 'NONE', #12253, #17301, #10396 ) ;
#4966 = CYLINDRICAL_SURFACE ( 'NONE', #3383, 0.2500000000000002220 ) ;
#4967 = EDGE_CURVE ( 'NONE', #8633, #5089, #942, .T. ) ;
#4968 = EDGE_CURVE ( 'NONE', #14892, #6732, #13429, .T. ) ;
#4969 = DIRECTION ( 'NONE',  ( -0.000000000000000000, -1.000000000000000000, -0.000000000000000000 ) ) ;
#4970 = VECTOR ( 'NONE', #17960, 1000.000000000000000 ) ;
#4971 = ORIENTED_EDGE ( 'NONE', *, *, #463, .F. ) ;
#4972 = EDGE_LOOP ( 'NONE', ( #10100, #3181, #12430, #305 ) ) ;
#4973 = ORIENTED_EDGE ( 'NONE', *, *, #15760, .T. ) ;
#4974 = DIRECTION ( 'NONE',  ( -1.000000000000000000, 0.000000000000000000, 0.000000000000000000 ) ) ;
#4975 = VECTOR ( 'NONE', #14617, 1000.000000000000000 ) ;
#4976 = DIRECTION ( 'NONE',  ( -1.000000000000000000, 0.000000000000000000, 0.000000000000000000 ) ) ;
#4977 = DIRECTION ( 'NONE',  ( 0.000000000000000000, -0.000000000000000000, -1.000000000000000000 ) ) ;
#4978 = ORIENTED_EDGE ( 'NONE', *, *, #20925, .F. ) ;
#4979 = ORIENTED_EDGE ( 'NONE', *, *, #21529, .T. ) ;
#4980 = DIRECTION ( 'NONE',  ( 0.000000000000000000, 0.000000000000000000, -1.000000000000000000 ) ) ;
#4981 = DIRECTION ( 'NONE',  ( 0.000000000000000000, -0.000000000000000000, -1.000000000000000000 ) ) ;
#4982 = EDGE_CURVE ( 'NONE', #18731, #17175, #16803, .T. ) ;
#4983 = LINE ( 'NONE', #18966, #2392 ) ;
#4984 = AXIS2_PLACEMENT_3D ( 'NONE', #4604, #11522, #21619 ) ;
#4985 = CYLINDRICAL_SURFACE ( 'NONE', #9166, 0.2999999999999999334 ) ;
#4986 = VERTEX_POINT ( 'NONE', #10210 ) ;
#4987 = CARTESIAN_POINT ( 'NONE',  ( -21.92816239687475743, 42.46645089659918426, 13.74999999999999822 ) ) ;
#4988 = FACE_OUTER_BOUND ( 'NONE', #8852, .T. ) ;
#4989 = DIRECTION ( 'NONE',  ( 1.000000000000000000, 0.000000000000000000, 6.123233995736764803E-17 ) ) ;
#4990 = FACE_OUTER_BOUND ( 'NONE', #1622, .T. ) ;
#4991 = ORIENTED_EDGE ( 'NONE', *, *, #1456, .T. ) ;
#4992 = DIRECTION ( 'NONE',  ( -0.000000000000000000, -0.000000000000000000, -1.000000000000000000 ) ) ;
#4993 = ADVANCED_FACE ( 'NONE', ( #13440 ), #24, .T. ) ;
#4994 = ORIENTED_EDGE ( 'NONE', *, *, #11958, .T. ) ;
#4995 = CARTESIAN_POINT ( 'NONE',  ( -8.638906393579159015, 41.51128595893310802, 69.94509975324525897 ) ) ;
#4996 = ADVANCED_FACE ( 'NONE', ( #10104 ), #13665, .T. ) ;
#4997 = FACE_OUTER_BOUND ( 'NONE', #9071, .T. ) ;
#4998 = ORIENTED_EDGE ( 'NONE', *, *, #19287, .F. ) ;
#4999 = AXIS2_PLACEMENT_3D ( 'NONE', #7119, #3533, #10467 ) ;
#5000 = ORIENTED_EDGE ( 'NONE', *, *, #3922, .F. ) ;
#5001 = VERTEX_POINT ( 'NONE', #9077 ) ;
#5002 = FACE_OUTER_BOUND ( 'NONE', #2950, .T. ) ;
#5003 = EDGE_CURVE ( 'NONE', #814, #5394, #15777, .T. ) ;
#5004 = DIRECTION ( 'NONE',  ( 1.000000000000000000, 0.000000000000000000, 0.000000000000000000 ) ) ;
#5005 = AXIS2_PLACEMENT_3D ( 'NONE', #17552, #2327, #646 ) ;
#5006 = CIRCLE ( 'NONE', #21445, 2.500000000000002220 ) ;
#5007 = ORIENTED_EDGE ( 'NONE', *, *, #18572, .T. ) ;
#5008 = DIRECTION ( 'NONE',  ( 2.107255972849994642E-16, 0.000000000000000000, 1.000000000000000000 ) ) ;
#5009 = ORIENTED_EDGE ( 'NONE', *, *, #1204, .T. ) ;
#5010 = ORIENTED_EDGE ( 'NONE', *, *, #7320, .F. ) ;
#5011 = CARTESIAN_POINT ( 'NONE',  ( 29.13662752439705272, 0.000000000000000000, 1.500000000000001332 ) ) ;
#5012 = DIRECTION ( 'NONE',  ( -1.000000000000000000, 0.000000000000000000, 0.000000000000000000 ) ) ;
#5013 = EDGE_CURVE ( 'NONE', #14923, #4893, #5407, .T. ) ;
#5014 = ORIENTED_EDGE ( 'NONE', *, *, #13731, .T. ) ;
#5015 = DIRECTION ( 'NONE',  ( 1.000000000000000000, 0.000000000000000000, -0.000000000000000000 ) ) ;
#5016 = LINE ( 'NONE', #1636, #643 ) ;
#5017 = CARTESIAN_POINT ( 'NONE',  ( 33.79999999999999716, -84.70000000000001705, 1.799999999999996048 ) ) ;
#5018 = CARTESIAN_POINT ( 'NONE',  ( 15.21174975910705918, 42.31054587065082728, 13.75000000000000000 ) ) ;
#5019 = EDGE_LOOP ( 'NONE', ( #19442, #2889, #3686, #14614 ) ) ;
#5020 = FACE_OUTER_BOUND ( 'NONE', #17538, .T. ) ;
#5021 = DIRECTION ( 'NONE',  ( 0.000000000000000000, 0.000000000000000000, 1.000000000000000000 ) ) ;
#5022 =( REPRESENTATION_RELATIONSHIP ('NONE','NONE', #561, #9142 ) REPRESENTATION_RELATIONSHIP_WITH_TRANSFORMATION ( #7399 )SHAPE_REPRESENTATION_RELATIONSHIP( ) );
#5023 = AXIS2_PLACEMENT_3D ( 'NONE', #18290, #19644, #13008 ) ;
#5024 = CIRCLE ( 'NONE', #4289, 0.5000000000000004441 ) ;
#5025 = DIRECTION ( 'NONE',  ( 1.000000000000000000, 0.000000000000000000, 0.000000000000000000 ) ) ;
#5026 = DIRECTION ( 'NONE',  ( 0.000000000000000000, 0.000000000000000000, 1.000000000000000000 ) ) ;
#5027 = ORIENTED_EDGE ( 'NONE', *, *, #10518, .F. ) ;
#5028 = DIRECTION ( 'NONE',  ( 1.000000000000000000, 0.000000000000000000, 0.000000000000000000 ) ) ;
#5029 = EDGE_CURVE ( 'NONE', #4526, #11406, #11987, .T. ) ;
#5030 = CARTESIAN_POINT ( 'NONE',  ( 33.79999999999999716, -84.70000000000001705, 2.931682674400803201E-15 ) ) ;
#5031 = ORIENTED_EDGE ( 'NONE', *, *, #5763, .T. ) ;
#5033 = EDGE_CURVE ( 'NONE', #10300, #15684, #344, .T. ) ;
#5032 = LINE ( 'NONE', #15424, #5339 ) ;
#5034 = DIRECTION ( 'NONE',  ( 1.000000000000000000, 0.000000000000000000, -0.000000000000000000 ) ) ;
#5035 = VERTEX_POINT ( 'NONE', #10435 ) ;
#5036 = ORIENTED_EDGE ( 'NONE', *, *, #7809, .F. ) ;
#5037 = FACE_OUTER_BOUND ( 'NONE', #20521, .T. ) ;
#5038 = AXIS2_PLACEMENT_3D ( 'NONE', #3955, #12749, #19277 ) ;
#5039 = AXIS2_PLACEMENT_3D ( 'NONE', #4050, #10863, #19942 ) ;
#5040 = ORIENTED_EDGE ( 'NONE', *, *, #15591, .T. ) ;
#5041 = CARTESIAN_POINT ( 'NONE',  ( 0.000000000000000000, 52.11873716947361856, 68.00000000000000000 ) ) ;
#5042 = ORIENTED_EDGE ( 'NONE', *, *, #9557, .T. ) ;
#5043 = FACE_OUTER_BOUND ( 'NONE', #21166, .T. ) ;
#5044 = LINE ( 'NONE', #8731, #7946 ) ;
#5045 = DIRECTION ( 'NONE',  ( -1.000000000000000000, -0.000000000000000000, -0.000000000000000000 ) ) ;
#5046 = ADVANCED_FACE ( 'NONE', ( #127 ), #449, .F. ) ;
#5047 = CARTESIAN_POINT ( 'NONE',  ( -1.774728116533986544, 42.31054587065082728, 31.80876104995653719 ) ) ;
#5048 = CARTESIAN_POINT ( 'NONE',  ( 14.96174975910707161, -51.61873716947361856, 68.25000000000000000 ) ) ;
#5049 = DIRECTION ( 'NONE',  ( -1.000000000000000000, 0.000000000000000000, 0.000000000000000000 ) ) ;
#5050 = CIRCLE ( 'NONE', #1831, 4.700000000000002842 ) ;
#5051 = DIRECTION ( 'NONE',  ( 0.000000000000000000, 0.000000000000000000, 1.000000000000000000 ) ) ;
#5052 = DIRECTION ( 'NONE',  ( 0.000000000000000000, 1.000000000000000000, 0.000000000000000000 ) ) ;
#5053 = DIRECTION ( 'NONE',  ( -1.000000000000000000, 0.000000000000000000, 0.000000000000000000 ) ) ;
#5054 = ADVANCED_FACE ( 'NONE', ( #12195 ), #3611, .F. ) ;
#5055 = CARTESIAN_POINT ( 'NONE',  ( -3.627054932750481964, -32.61873716947361856, 7.321391277662001151 ) ) ;
#5056 = VERTEX_POINT ( 'NONE', #3827 ) ;
#5057 = DIRECTION ( 'NONE',  ( 0.000000000000000000, 1.000000000000000000, 0.000000000000000000 ) ) ;
#5058 = DIRECTION ( 'NONE',  ( -0.000000000000000000, -0.000000000000000000, -1.000000000000000000 ) ) ;
#5059 = ORIENTED_EDGE ( 'NONE', *, *, #4308, .F. ) ;
#5060 = CARTESIAN_POINT ( 'NONE',  ( 1.824728116533979261, 42.36054587065083155, 51.70876104995653577 ) ) ;
#5061 = SHAPE_DEFINITION_REPRESENTATION ( #1428, #12850 ) ;
#5062 = AXIS2_PLACEMENT_3D ( 'NONE', #20201, #16400, #6464 ) ;
#5063 = VERTEX_POINT ( 'NONE', #13990 ) ;
#5064 = CIRCLE ( 'NONE', #16827, 0.05000000000000143219 ) ;
#5065 = ORIENTED_EDGE ( 'NONE', *, *, #973, .F. ) ;
#5066 = VERTEX_POINT ( 'NONE', #228 ) ;
#5067 = EDGE_CURVE ( 'NONE', #19115, #6081, #6665, .T. ) ;
#5068 = DIRECTION ( 'NONE',  ( -0.000000000000000000, -0.000000000000000000, -1.000000000000000000 ) ) ;
#5069 = LINE ( 'NONE', #3380, #13461 ) ;
#5070 = VECTOR ( 'NONE', #4294, 1000.000000000000000 ) ;
#5071 = ADVANCED_FACE ( 'NONE', ( #20943 ), #20841, .T. ) ;
#5072 = CARTESIAN_POINT ( 'NONE',  ( 9.141460742840918030, 33.43424481021354921, 7.321391277662001151 ) ) ;
#5073 = ORIENTED_EDGE ( 'NONE', *, *, #6329, .T. ) ;
#5074 = VECTOR ( 'NONE', #20948, 1000.000000000000000 ) ;
#5075 = FACE_OUTER_BOUND ( 'NONE', #20446, .T. ) ;
#5076 = AXIS2_PLACEMENT_3D ( 'NONE', #6734, #11953, #317 ) ;
#5077 = LINE ( 'NONE', #18713, #13980 ) ;
#5078 = DIRECTION ( 'NONE',  ( -2.107255972849994642E-16, 0.000000000000000000, -1.000000000000000000 ) ) ;
#5079 = CARTESIAN_POINT ( 'NONE',  ( -29.13662752439705272, -4.700000000000000178, 3.799999999999999822 ) ) ;
#5080 = CARTESIAN_POINT ( 'NONE',  ( 17.95292532278785913, 38.74634676501045760, 13.99999999999999822 ) ) ;
#5081 = ORIENTED_EDGE ( 'NONE', *, *, #10478, .F. ) ;
#5082 = ORIENTED_EDGE ( 'NONE', *, *, #62, .F. ) ;
#5083 = VERTEX_POINT ( 'NONE', #5627 ) ;
#5084 = CARTESIAN_POINT ( 'NONE',  ( -30.07540678000427548, 63.74634676501045050, 7.200000000000000178 ) ) ;
#5085 = CARTESIAN_POINT ( 'NONE',  ( -1.724728116533986721, 43.31054587065082728, 33.76679706732591058 ) ) ;
#5086 = ORIENTED_EDGE ( 'NONE', *, *, #14754, .T. ) ;
#5087 = ADVANCED_FACE ( 'NONE', ( #8752 ), #5598, .T. ) ;
#5088 = CARTESIAN_POINT ( 'NONE',  ( -4.127054932750482408, -32.93424481021354921, 68.00000000000000000 ) ) ;
#5089 = VERTEX_POINT ( 'NONE', #17347 ) ;
#5090 = TOROIDAL_SURFACE ( 'NONE', #20466, 6.800000000000001599, 0.2999999999999999889 ) ;
#5091 = CIRCLE ( 'NONE', #11514, 0.2500000000000002220 ) ;
#5092 = ORIENTED_EDGE ( 'NONE', *, *, #16104, .F. ) ;
#5093 = CARTESIAN_POINT ( 'NONE',  ( -15.95292532278785913, 52.39333383871510108, 13.79999999999999893 ) ) ;
#5094 = ADVANCED_FACE ( 'NONE', ( #7086 ), #13883, .T. ) ;
#5095 = CARTESIAN_POINT ( 'NONE',  ( -14.71174975910705029, 0.000000000000000000, 68.50000000000000000 ) ) ;
#5096 = CARTESIAN_POINT ( 'NONE',  ( -29.37540678000427619, -5.000000000000000000, 7.200000000000000178 ) ) ;
#5097 = ORIENTED_EDGE ( 'NONE', *, *, #4666, .F. ) ;
#5098 = CARTESIAN_POINT ( 'NONE',  ( -21.91689697940243775, 45.66657467514198743, 68.50000000000000000 ) ) ;
#5099 = CARTESIAN_POINT ( 'NONE',  ( -11.67890639357915816, 42.46645089659918426, 74.06027860057353962 ) ) ;
#5100 = DIRECTION ( 'NONE',  ( 0.000000000000000000, -1.000000000000000000, 0.000000000000000000 ) ) ;
#5101 = DIRECTION ( 'NONE',  ( 0.000000000000000000, 0.000000000000000000, 1.000000000000000000 ) ) ;
#5102 = DIRECTION ( 'NONE',  ( 0.000000000000000000, -0.000000000000000000, -1.000000000000000000 ) ) ;
#5103 = ORIENTED_EDGE ( 'NONE', *, *, #10202, .F. ) ;
#5104 = LINE ( 'NONE', #14939, #11620 ) ;
#5105 = CARTESIAN_POINT ( 'NONE',  ( 0.000000000000000000, 51.61873716947361856, 14.00000000000000000 ) ) ;
#5106 = AXIS2_PLACEMENT_3D ( 'NONE', #767, #9624, #13058 ) ;
#5107 = ORIENTED_EDGE ( 'NONE', *, *, #20585, .F. ) ;
#5108 = DIRECTION ( 'NONE',  ( -1.000000000000000000, 0.000000000000000000, 0.000000000000000000 ) ) ;
#5109 = DIRECTION ( 'NONE',  ( 0.000000000000000000, 0.000000000000000000, 1.000000000000000000 ) ) ;
#5110 = CIRCLE ( 'NONE', #17893, 0.1000000000000028644 ) ;
#5111 = DIRECTION ( 'NONE',  ( 0.000000000000000000, 0.000000000000000000, 1.000000000000000000 ) ) ;
#5112 = ORIENTED_EDGE ( 'NONE', *, *, #406, .T. ) ;
#5113 = VERTEX_POINT ( 'NONE', #10650 ) ;
#5114 = ORIENTED_EDGE ( 'NONE', *, *, #11639, .F. ) ;
#5115 = DIRECTION ( 'NONE',  ( 0.000000000000000000, 0.000000000000000000, 1.000000000000000000 ) ) ;
#5116 = DIRECTION ( 'NONE',  ( -0.000000000000000000, 1.000000000000000000, -0.000000000000000000 ) ) ;
#5117 = EDGE_CURVE ( 'NONE', #1711, #9267, #20730, .T. ) ;
#5118 = CARTESIAN_POINT ( 'NONE',  ( 3.127054932750481964, -32.61873716947361856, 42.50000000000000711 ) ) ;
#5119 = ORIENTED_EDGE ( 'NONE', *, *, #7063, .F. ) ;
#5120 = CARTESIAN_POINT ( 'NONE',  ( 17.95292532278785913, 0.000000000000000000, 109.6002446535588319 ) ) ;
#5121 = ORIENTED_EDGE ( 'NONE', *, *, #20385, .F. ) ;
#5122 = CARTESIAN_POINT ( 'NONE',  ( 30.19999999999999574, 70.29999999999999716, 3.992348565220370405E-15 ) ) ;
#5123 = EDGE_CURVE ( 'NONE', #5378, #12212, #1649, .T. ) ;
#5124 = EDGE_CURVE ( 'NONE', #10124, #5205, #14142, .T. ) ;
#5125 = EDGE_LOOP ( 'NONE', ( #4457, #10045, #4891, #6192 ) ) ;
#5126 = PLANE ( 'NONE',  #13857 ) ;
#5127 = ADVANCED_FACE ( 'NONE', ( #15878 ), #556, .F. ) ;
#5128 = DIRECTION ( 'NONE',  ( 0.000000000000000000, -0.000000000000000000, 1.000000000000000000 ) ) ;
#5129 = DIRECTION ( 'NONE',  ( 0.000000000000000000, -1.000000000000000000, 0.000000000000000000 ) ) ;
#5130 = VERTEX_POINT ( 'NONE', #12857 ) ;
#5131 = CARTESIAN_POINT ( 'NONE',  ( 23.02398829872514341, 2.211005166399008459, 13.20000000000005791 ) ) ;
#5132 = CARTESIAN_POINT ( 'NONE',  ( -3.127054932750481964, 32.11873716947361856, 68.00000000000000000 ) ) ;
#5133 = FACE_OUTER_BOUND ( 'NONE', #3595, .T. ) ;
#5134 = FACE_OUTER_BOUND ( 'NONE', #17700, .T. ) ;
#5135 = ORIENTED_EDGE ( 'NONE', *, *, #13056, .T. ) ;
#5136 = DIRECTION ( 'NONE',  ( -0.000000000000000000, -1.000000000000000000, -0.000000000000000000 ) ) ;
#5137 = LINE ( 'NONE', #6499, #1647 ) ;
#5138 = ORIENTED_EDGE ( 'NONE', *, *, #4116, .T. ) ;
#5139 = DIRECTION ( 'NONE',  ( 0.000000000000000000, 0.000000000000000000, 1.000000000000000000 ) ) ;
#5140 = EDGE_CURVE ( 'NONE', #15087, #16789, #200, .T. ) ;
#5141 = DIRECTION ( 'NONE',  ( 1.000000000000000000, 0.000000000000000000, 0.000000000000000000 ) ) ;
#5142 = ORIENTED_EDGE ( 'NONE', *, *, #16497, .F. ) ;
#5143 = CARTESIAN_POINT ( 'NONE',  ( 1.774728116533979438, 42.36054587065083155, 47.70876104995654288 ) ) ;
#5144 = EDGE_LOOP ( 'NONE', ( #7513, #7102, #17750, #4759 ) ) ;
#5145 = EDGE_CURVE ( 'NONE', #9228, #444, #14653, .T. ) ;
#5146 = DIRECTION ( 'NONE',  ( 0.000000000000000000, 1.000000000000000000, 0.000000000000000000 ) ) ;
#5147 = EDGE_LOOP ( 'NONE', ( #15006, #14341, #2121, #20232 ) ) ;
#5148 = DIRECTION ( 'NONE',  ( 0.000000000000000000, -1.000000000000000000, 0.000000000000000000 ) ) ;
#5149 = ADVANCED_FACE ( 'NONE', ( #4150 ), #4374, .T. ) ;
#5150 = AXIS2_PLACEMENT_3D ( 'NONE', #2828, #18362, #7875 ) ;
#5151 = DIRECTION ( 'NONE',  ( 0.000000000000000000, 0.000000000000000000, -1.000000000000000000 ) ) ;
#5152 = DIRECTION ( 'NONE',  ( 0.000000000000000000, 0.000000000000000000, 1.000000000000000000 ) ) ;
#5153 = EDGE_CURVE ( 'NONE', #12260, #8060, #17675, .T. ) ;
#5154 = DIRECTION ( 'NONE',  ( 1.000000000000000000, 0.000000000000000000, 0.000000000000000000 ) ) ;
#5155 = DIRECTION ( 'NONE',  ( -2.107255972849994642E-16, 0.000000000000000000, -1.000000000000000000 ) ) ;
#5156 = CYLINDRICAL_SURFACE ( 'NONE', #3924, 0.5000000000000004441 ) ;
#5157 = CARTESIAN_POINT ( 'NONE',  ( -27.37540678000427974, -5.683640910026986681, 13.50000000000000000 ) ) ;
#5158 = AXIS2_PLACEMENT_3D ( 'NONE', #3567, #16630, #5576 ) ;
#5159 = DIRECTION ( 'NONE',  ( 0.9729678061520339316, 0.2309407893632007824, 0.000000000000000000 ) ) ;
#5160 = DIRECTION ( 'NONE',  ( -1.000000000000000000, 0.000000000000000000, 0.000000000000000000 ) ) ;
#5161 = EDGE_LOOP ( 'NONE', ( #2233, #13724, #18262, #10625 ) ) ;
#5162 = EDGE_CURVE ( 'NONE', #17318, #5997, #7858, .T. ) ;
#5163 = CARTESIAN_POINT ( 'NONE',  ( 0.000000000000000000, -52.39333383871510108, 13.79999999999999893 ) ) ;
#5164 = LINE ( 'NONE', #17006, #8823 ) ;
#5165 = VECTOR ( 'NONE', #4934, 1000.000000000000114 ) ;
#5166 = ORIENTED_EDGE ( 'NONE', *, *, #15789, .F. ) ;
#5167 = AXIS2_PLACEMENT_3D ( 'NONE', #8130, #11571, #13257 ) ;
#5168 = ORIENTED_EDGE ( 'NONE', *, *, #21884, .F. ) ;
#5169 = FACE_OUTER_BOUND ( 'NONE', #6126, .T. ) ;
#5170 = DIRECTION ( 'NONE',  ( 0.000000000000000000, 0.000000000000000000, 1.000000000000000000 ) ) ;
#5171 = EDGE_CURVE ( 'NONE', #808, #11153, #10971, .T. ) ;
#5172 = ORIENTED_EDGE ( 'NONE', *, *, #20907, .F. ) ;
#5173 = PRESENTATION_STYLE_ASSIGNMENT (( #1468 ) ) ;
#5174 = ORIENTED_EDGE ( 'NONE', *, *, #13644, .F. ) ;
#5175 = ORIENTED_EDGE ( 'NONE', *, *, #6398, .F. ) ;
#5176 = EDGE_LOOP ( 'NONE', ( #13608, #22158, #18759, #19831, #12843, #6196 ) ) ;
#5177 = ADVANCED_FACE ( 'NONE', ( #9410 ), #14766, .T. ) ;
#5178 = DIRECTION ( 'NONE',  ( 0.000000000000000000, 0.000000000000000000, -1.000000000000000000 ) ) ;
#5179 = CARTESIAN_POINT ( 'NONE',  ( -1.824728116533986810, 42.36054587065083155, 29.71679706732590631 ) ) ;
#5180 = DIRECTION ( 'NONE',  ( 1.000000000000000000, 0.000000000000000000, 0.000000000000000000 ) ) ;
#5181 = AXIS2_PLACEMENT_3D ( 'NONE', #18714, #18375, #8219 ) ;
#5182 = FACE_OUTER_BOUND ( 'NONE', #2940, .T. ) ;
#5183 = CARTESIAN_POINT ( 'NONE',  ( 14.96174975910705918, 41.81054587065082728, 13.75000000000000000 ) ) ;
#5184 = CYLINDRICAL_SURFACE ( 'NONE', #2557, 0.2999999999999999334 ) ;
#5185 = FACE_OUTER_BOUND ( 'NONE', #7564, .T. ) ;
#5186 = CARTESIAN_POINT ( 'NONE',  ( -17.45292532278785913, -50.11873716947361856, 68.00000000000000000 ) ) ;
#5187 = CARTESIAN_POINT ( 'NONE',  ( 25.37540678000427263, 66.94634676501046044, 13.50000000000000000 ) ) ;
#5188 = ORIENTED_EDGE ( 'NONE', *, *, #18989, .T. ) ;
#5189 = ORIENTED_EDGE ( 'NONE', *, *, #4018, .T. ) ;
#5190 = CARTESIAN_POINT ( 'NONE',  ( 25.37540678000427263, 63.74634676501045050, 7.500000000000000000 ) ) ;
#5191 = PRESENTATION_STYLE_ASSIGNMENT (( #20523 ) ) ;
#5193 = ADVANCED_FACE ( 'NONE', ( #6182 ), #17371, .T. ) ;
#5192 = DIRECTION ( 'NONE',  ( 0.000000000000000000, 0.000000000000000000, 1.000000000000000000 ) ) ;
#5194 = ORIENTED_EDGE ( 'NONE', *, *, #6674, .T. ) ;
#5195 = ADVANCED_FACE ( 'NONE', ( #2683 ), #217, .T. ) ;
#5196 = ADVANCED_FACE ( 'NONE', ( #12965 ), #9517, .F. ) ;
#5197 = AXIS2_PLACEMENT_3D ( 'NONE', #3778, #17004, #20801 ) ;
#5198 = CARTESIAN_POINT ( 'NONE',  ( 17.95292532278785913, 0.000000000000000000, 68.00000000000000000 ) ) ;
#5199 = AXIS2_PLACEMENT_3D ( 'NONE', #12047, #17102, #5028 ) ;
#5200 = DIRECTION ( 'NONE',  ( -1.000000000000000000, 0.000000000000000000, 0.000000000000000000 ) ) ;
#5201 = CARTESIAN_POINT ( 'NONE',  ( -23.02398829872513986, -2.157133568460768647, 42.50000000000000000 ) ) ;
#5202 = DIRECTION ( 'NONE',  ( 0.000000000000000000, 0.000000000000000000, 1.000000000000000000 ) ) ;
#5203 = DIRECTION ( 'NONE',  ( 1.000000000000000000, 0.000000000000000000, -0.000000000000000000 ) ) ;
#5204 = AXIS2_PLACEMENT_3D ( 'NONE', #17581, #2246, #15879 ) ;
#5205 = VERTEX_POINT ( 'NONE', #5850 ) ;
#5206 = DIRECTION ( 'NONE',  ( 1.000000000000000000, 0.000000000000000000, 0.000000000000000000 ) ) ;
#5207 = CYLINDRICAL_SURFACE ( 'NONE', #7134, 0.2500000000000002220 ) ;
#5208 = FACE_OUTER_BOUND ( 'NONE', #14813, .T. ) ;
#5209 = DIRECTION ( 'NONE',  ( 0.000000000000000000, 0.000000000000000000, 1.000000000000000000 ) ) ;
#5210 = CARTESIAN_POINT ( 'NONE',  ( -14.71174975910705029, 51.86873716947361856, 109.6002446535588319 ) ) ;
#5211 = ORIENTED_EDGE ( 'NONE', *, *, #6753, .T. ) ;
#5212 = PRODUCT_DEFINITION ( 'UNKNOWN', '', #19435, #22082 ) ;
#5213 = CARTESIAN_POINT ( 'NONE',  ( 0.000000000000000000, 52.10286008774954780, 13.87500000000000000 ) ) ;
#5214 = ADVANCED_FACE ( 'NONE', ( #2807 ), #20965, .T. ) ;
#5215 = AXIS2_PLACEMENT_3D ( 'NONE', #5904, #16948, #11909 ) ;
#5216 = VECTOR ( 'NONE', #590, 1000.000000000000000 ) ;
#5217 = CIRCLE ( 'NONE', #7009, 0.3000000000000016542 ) ;
#5218 = EDGE_LOOP ( 'NONE', ( #13090, #4517, #4096, #16617 ) ) ;
#5219 = LINE ( 'NONE', #12231, #17897 ) ;
#5220 = CARTESIAN_POINT ( 'NONE',  ( 0.000000000000000000, 0.000000000000000000, 68.50000000000000000 ) ) ;
#5221 = CARTESIAN_POINT ( 'NONE',  ( 0.000000000000000000, 5.000000000000000000, 7.500000000000000000 ) ) ;
#5222 = EDGE_LOOP ( 'NONE', ( #8586, #14321, #2761, #9094, #21705, #12029, #8332 ) ) ;
#5223 = VERTEX_POINT ( 'NONE', #17900 ) ;
#5224 = ORIENTED_EDGE ( 'NONE', *, *, #20474, .T. ) ;
#5225 = FACE_OUTER_BOUND ( 'NONE', #21938, .T. ) ;
#5226 = DIRECTION ( 'NONE',  ( -0.000000000000000000, -0.000000000000000000, -1.000000000000000000 ) ) ;
#5227 = EDGE_CURVE ( 'NONE', #22131, #21935, #18123, .T. ) ;
#5228 = DIRECTION ( 'NONE',  ( 0.000000000000000000, 0.000000000000000000, 1.000000000000000000 ) ) ;
#5229 = ADVANCED_FACE ( 'NONE', ( #16446 ), #10860, .F. ) ;
#5230 = DIRECTION ( 'NONE',  ( 1.000000000000000000, 0.000000000000000000, 0.000000000000000000 ) ) ;
#5231 = TOROIDAL_SURFACE ( 'NONE', #1265, 0.05000000000000000278, 0.05000000000000000278 ) ;
#5232 = ORIENTED_EDGE ( 'NONE', *, *, #2585, .T. ) ;
#5233 = DIRECTION ( 'NONE',  ( -0.000000000000000000, -0.000000000000000000, -1.000000000000000000 ) ) ;
#5234 = AXIS2_PLACEMENT_3D ( 'NONE', #21275, #18344, #9516 ) ;
#5235 = AXIS2_PLACEMENT_3D ( 'NONE', #9887, #19971, #10216 ) ;
#5236 = VECTOR ( 'NONE', #12649, 1000.000000000000000 ) ;
#5237 = EDGE_LOOP ( 'NONE', ( #881, #7667, #12836, #3365 ) ) ;
#5238 = CARTESIAN_POINT ( 'NONE',  ( -23.02398829872536368, -3.053353875533148187, 13.54966661417588547 ) ) ;
#5239 = DIRECTION ( 'NONE',  ( 0.000000000000000000, 0.000000000000000000, 1.000000000000000000 ) ) ;
#5240 = DIRECTION ( 'NONE',  ( 1.000000000000000000, 0.000000000000000000, 0.000000000000000000 ) ) ;
#5241 = CARTESIAN_POINT ( 'NONE',  ( -23.32398829872514057, -3.528912754968629439, 13.50000000000000000 ) ) ;
#5242 = ORIENTED_EDGE ( 'NONE', *, *, #18803, .T. ) ;
#5243 = CARTESIAN_POINT ( 'NONE',  ( 23.02398829872513986, 3.005406968599039441, 13.74590378743891250 ) ) ;
#5244 = DIRECTION ( 'NONE',  ( 0.000000000000000000, 0.000000000000000000, 1.000000000000000000 ) ) ;
#5245 = CARTESIAN_POINT ( 'NONE',  ( -31.50000000000002132, 71.00000000000001421, 3.500000000000000000 ) ) ;
#5246 = CARTESIAN_POINT ( 'NONE',  ( -21.92816239687475743, 42.46645089659918426, 68.50000000000000000 ) ) ;
#5247 = ORIENTED_EDGE ( 'NONE', *, *, #12958, .F. ) ;
#5248 = ADVANCED_FACE ( 'NONE', ( #678 ), #4160, .F. ) ;
#5249 = CIRCLE ( 'NONE', #8096, 5.000000000000004441 ) ;
#5250 = VECTOR ( 'NONE', #8494, 1000.000000000000000 ) ;
#5251 = DIRECTION ( 'NONE',  ( 1.000000000000000000, 0.000000000000000000, 0.000000000000000000 ) ) ;
#5252 = AXIS2_PLACEMENT_3D ( 'NONE', #18345, #13538, #8187 ) ;
#5253 = DIRECTION ( 'NONE',  ( 0.000000000000000000, 0.000000000000000000, 1.000000000000000000 ) ) ;
#5254 = ORIENTED_EDGE ( 'NONE', *, *, #16614, .F. ) ;
#5255 = AXIS2_PLACEMENT_3D ( 'NONE', #21286, #18137, #9651 ) ;
#5256 = EDGE_CURVE ( 'NONE', #10046, #17759, #19470, .T. ) ;
#5257 = DIRECTION ( 'NONE',  ( -0.000000000000000000, 0.000000000000000000, 1.000000000000000000 ) ) ;
#5258 = VERTEX_POINT ( 'NONE', #5047 ) ;
#5259 = DIRECTION ( 'NONE',  ( -1.000000000000000000, -0.000000000000000000, 0.000000000000000000 ) ) ;
#5260 = ORIENTED_EDGE ( 'NONE', *, *, #15194, .T. ) ;
#5261 = CIRCLE ( 'NONE', #14877, 2.000000000000001776 ) ;
#5262 = AXIS2_PLACEMENT_3D ( 'NONE', #9353, #16159, #7678 ) ;
#5263 = VECTOR ( 'NONE', #846, 1000.000000000000000 ) ;
#5264 = CARTESIAN_POINT ( 'NONE',  ( -34.70000000000000284, 85.00000000000000000, 0.6000000000000033085 ) ) ;
#5265 = EDGE_LOOP ( 'NONE', ( #6307, #1889, #4106, #10509, #20237, #10454, #22118, #9174, #7779, #8884, #6322, #839, #17236, #8913, #7324, #12786, #13406, #19497, #6204, #3037, #7290, #21475, #1825, #13191, #10207, #15791, #4612, #17460, #20773, #13807 ) ) ;
#5266 = CARTESIAN_POINT ( 'NONE',  ( -29.13662752439705272, 0.000000000000000000, 7.500000000000000000 ) ) ;
#5267 = CIRCLE ( 'NONE', #15258, 0.2500000000000002220 ) ;
#5268 = DIRECTION ( 'NONE',  ( 0.000000000000000000, 1.000000000000000000, -0.000000000000000000 ) ) ;
#5269 = DIRECTION ( 'NONE',  ( 1.000000000000000000, 0.000000000000000000, 0.000000000000000000 ) ) ;
#5270 = EDGE_CURVE ( 'NONE', #20330, #20326, #21685, .T. ) ;
#5271 = CARTESIAN_POINT ( 'NONE',  ( 27.37540678000427974, -10.94079601157914716, 13.79999999999999893 ) ) ;
#5272 = CARTESIAN_POINT ( 'NONE',  ( 1.724728116533979616, 42.36054587065083155, 51.80876104995653719 ) ) ;
#5273 = AXIS2_PLACEMENT_3D ( 'NONE', #7217, #15800, #256 ) ;
#5274 = LINE ( 'NONE', #20921, #2590 ) ;
#5275 = VECTOR ( 'NONE', #16199, 1000.000000000000000 ) ;
#5276 = CIRCLE ( 'NONE', #12724, 1.000000000000000000 ) ;
#5277 = EDGE_CURVE ( 'NONE', #19227, #11507, #20046, .T. ) ;
#5278 = ORIENTED_EDGE ( 'NONE', *, *, #4471, .T. ) ;
#5279 = ADVANCED_FACE ( 'NONE', ( #3024 ), #3136, .T. ) ;
#5280 = CARTESIAN_POINT ( 'NONE',  ( -1.724728116533986721, 42.36054587065083155, 43.75876104995654003 ) ) ;
#5281 = CARTESIAN_POINT ( 'NONE',  ( 29.50000000000002132, -2.473451120191013430, 0.2999999999999947153 ) ) ;
#5282 = EDGE_CURVE ( 'NONE', #5035, #5552, #935, .T. ) ;
#5283 = VECTOR ( 'NONE', #8991, 1000.000000000000000 ) ;
#5284 = DIRECTION ( 'NONE',  ( 0.000000000000000000, 0.000000000000000000, 1.000000000000000000 ) ) ;
#5285 = DIRECTION ( 'NONE',  ( -1.000000000000000000, 0.000000000000000000, 0.000000000000000000 ) ) ;
#5286 = ORIENTED_EDGE ( 'NONE', *, *, #17436, .F. ) ;
#5287 = AXIS2_PLACEMENT_3D ( 'NONE', #14492, #21242, #17129 ) ;
#5288 = ORIENTED_EDGE ( 'NONE', *, *, #21991, .T. ) ;
#5289 = FACE_OUTER_BOUND ( 'NONE', #7620, .T. ) ;
#5290 = EDGE_CURVE ( 'NONE', #833, #17644, #4711, .T. ) ;
#5291 = CARTESIAN_POINT ( 'NONE',  ( 27.13561920550106521, -5.281294294914825826, -8.673617379884035472E-16 ) ) ;
#5292 = ORIENTED_EDGE ( 'NONE', *, *, #20301, .T. ) ;
#5293 =( LENGTH_UNIT ( ) NAMED_UNIT ( * ) SI_UNIT ( .MILLI., .METRE. ) );
#5294 = CARTESIAN_POINT ( 'NONE',  ( -1.824728116533986810, 42.36054587065083155, 39.80876104995653719 ) ) ;
#5295 = ORIENTED_EDGE ( 'NONE', *, *, #17851, .T. ) ;
#5296 = AXIS2_PLACEMENT_3D ( 'NONE', #4786, #4896, #18543 ) ;
#5297 = VECTOR ( 'NONE', #7378, 1000.000000000000000 ) ;
#5298 = AXIS2_PLACEMENT_3D ( 'NONE', #2669, #21712, #11509 ) ;
#5299 = EDGE_LOOP ( 'NONE', ( #14131, #10023, #4114, #10319 ) ) ;
#5300 = DIRECTION ( 'NONE',  ( -0.000000000000000000, -0.000000000000000000, -1.000000000000000000 ) ) ;
#5301 = ADVANCED_FACE ( 'NONE', ( #1670 ), #18240, .T. ) ;
#5302 = DIRECTION ( 'NONE',  ( -1.000000000000000000, 0.000000000000000000, -0.000000000000000000 ) ) ;
#5303 = AXIS2_PLACEMENT_3D ( 'NONE', #8357, #17185, #3551 ) ;
#5304 = DIRECTION ( 'NONE',  ( 0.000000000000000000, 0.000000000000000000, 1.000000000000000000 ) ) ;
#5305 = VECTOR ( 'NONE', #15365, 1000.000000000000000 ) ;
#5306 = CARTESIAN_POINT ( 'NONE',  ( -30.07540678000427548, -6.000000000000000000, 7.200000000000000178 ) ) ;
#5307 = CIRCLE ( 'NONE', #22091, 0.2999999999999999334 ) ;
#5308 = CARTESIAN_POINT ( 'NONE',  ( -23.32398829872514057, 7.118794219358020148E-15, 13.79999999999999893 ) ) ;
#5309 = DIRECTION ( 'NONE',  ( 0.000000000000000000, 0.000000000000000000, -1.000000000000000000 ) ) ;
#5310 = DIRECTION ( 'NONE',  ( 0.000000000000000000, 0.000000000000000000, 1.000000000000000000 ) ) ;
#5311 = FACE_OUTER_BOUND ( 'NONE', #9235, .T. ) ;
#5312 = CARTESIAN_POINT ( 'NONE',  ( 1.724728116533979838, 43.26054587065083012, 37.66679706732590915 ) ) ;
#5313 = EDGE_CURVE ( 'NONE', #21235, #16141, #13204, .T. ) ;
#5314 = AXIS2_PLACEMENT_3D ( 'NONE', #10021, #20310, #6667 ) ;
#5315 = VECTOR ( 'NONE', #9264, 1000.000000000000000 ) ;
#5316 = ORIENTED_EDGE ( 'NONE', *, *, #3503, .F. ) ;
#5317 = VERTEX_POINT ( 'NONE', #8512 ) ;
#5318 = CARTESIAN_POINT ( 'NONE',  ( -31.26086011588028057, 83.95073979834609190, 68.25000000000000000 ) ) ;
#5319 = EDGE_CURVE ( 'NONE', #21932, #1327, #18685, .T. ) ;
#5320 =( LENGTH_UNIT ( ) NAMED_UNIT ( * ) SI_UNIT ( .MILLI., .METRE. ) );
#5321 = CARTESIAN_POINT ( 'NONE',  ( 1.774728116533979883, 43.26054587065083012, 29.66679706732590560 ) ) ;
#5322 = ORIENTED_EDGE ( 'NONE', *, *, #1610, .F. ) ;
#5323 = AXIS2_PLACEMENT_3D ( 'NONE', #2329, #14075, #15857 ) ;
#5324 = AXIS2_PLACEMENT_3D ( 'NONE', #6423, #898, #17809 ) ;
#5325 = CIRCLE ( 'NONE', #995, 0.2999999999999999334 ) ;
#5326 = CARTESIAN_POINT ( 'NONE',  ( 33.19999999999999574, 84.70000000000001705, 78.79999999999999716 ) ) ;
#5327 = CARTESIAN_POINT ( 'NONE',  ( 0.000000000000000000, 32.11873716947361856, 42.50000000000000711 ) ) ;
#5328 = AXIS2_PLACEMENT_3D ( 'NONE', #16174, #19893, #11152 ) ;
#5329 = CARTESIAN_POINT ( 'NONE',  ( -28.87540678000427619, 0.000000000000000000, 13.50000000000000000 ) ) ;
#5330 = ORIENTED_EDGE ( 'NONE', *, *, #10091, .F. ) ;
#5331 = LINE ( 'NONE', #3409, #17023 ) ;
#5332 = CARTESIAN_POINT ( 'NONE',  ( -1.724728116533986721, 42.31054587065082728, 41.66679706732590915 ) ) ;
#5333 = ADVANCED_FACE ( 'NONE', ( #1333 ), #14163, .T. ) ;
#5334 = DIRECTION ( 'NONE',  ( 4.336808689941893885E-15, 0.000000000000000000, 1.000000000000000000 ) ) ;
#5335 = VECTOR ( 'NONE', #20129, 1000.000000000000000 ) ;
#5336 = DIRECTION ( 'NONE',  ( 0.000000000000000000, 0.000000000000000000, 1.000000000000000000 ) ) ;
#5337 = CARTESIAN_POINT ( 'NONE',  ( -29.37540678000427619, 6.000000000000000000, 7.500000000000000000 ) ) ;
#5338 = FACE_OUTER_BOUND ( 'NONE', #19332, .T. ) ;
#5339 = VECTOR ( 'NONE', #16981, 1000.000000000000000 ) ;
#5340 = ORIENTED_EDGE ( 'NONE', *, *, #8282, .T. ) ;
#5341 = LINE ( 'NONE', #3419, #4340 ) ;
#5342 = DIRECTION ( 'NONE',  ( 0.000000000000000000, 0.000000000000000000, 1.000000000000000000 ) ) ;
#5343 = ORIENTED_EDGE ( 'NONE', *, *, #9449, .F. ) ;
#5344 = EDGE_LOOP ( 'NONE', ( #21632, #17523, #21984, #17636 ) ) ;
#5345 = ORIENTED_EDGE ( 'NONE', *, *, #15088, .F. ) ;
#5346 = DIRECTION ( 'NONE',  ( 1.000000000000000000, 0.000000000000000000, 0.000000000000000000 ) ) ;
#5347 = CARTESIAN_POINT ( 'NONE',  ( -14.96174975910705207, -51.61873716947361856, 68.00000000000000000 ) ) ;
#5348 = EDGE_CURVE ( 'NONE', #18368, #17156, #1661, .T. ) ;
#5349 = CARTESIAN_POINT ( 'NONE',  ( 0.000000000000000000, -38.74634676501045760, 13.79999999999999893 ) ) ;
#5350 = CARTESIAN_POINT ( 'NONE',  ( -1.724728116533986721, 43.26054587065083012, 35.80876104995653009 ) ) ;
#5351 = AXIS2_PLACEMENT_3D ( 'NONE', #9003, #7326, #17057 ) ;
#5352 = ORIENTED_EDGE ( 'NONE', *, *, #2991, .F. ) ;
#5353 = DIRECTION ( 'NONE',  ( 0.000000000000000000, 0.000000000000000000, 1.000000000000000000 ) ) ;
#5354 = CIRCLE ( 'NONE', #19625, 0.05000000000000143219 ) ;
#5355 = ORIENTED_EDGE ( 'NONE', *, *, #2679, .F. ) ;
#5356 = DIRECTION ( 'NONE',  ( -0.000000000000000000, -0.000000000000000000, -1.000000000000000000 ) ) ;
#5357 = CARTESIAN_POINT ( 'NONE',  ( -23.02398829872513986, 3.528912754968630328, 13.79999999999999893 ) ) ;
#5358 = CARTESIAN_POINT ( 'NONE',  ( -29.13662752439705272, 0.000000000000000000, 3.799999999999999822 ) ) ;
#5359 = CARTESIAN_POINT ( 'NONE',  ( -9.718906393579157310, 41.42245079618239600, 68.06527860057354928 ) ) ;
#5360 = EDGE_LOOP ( 'NONE', ( #18587, #18497, #5449, #20084 ) ) ;
#5361 = DIRECTION ( 'NONE',  ( 1.000000000000000000, 0.000000000000000000, 0.000000000000000000 ) ) ;
#5362 = FACE_OUTER_BOUND ( 'NONE', #13675, .T. ) ;
#5363 = EDGE_CURVE ( 'NONE', #16845, #16208, #6406, .T. ) ;
#5364 = DIRECTION ( 'NONE',  ( 1.000000000000000000, -0.000000000000000000, -0.000000000000000000 ) ) ;
#5365 = CARTESIAN_POINT ( 'NONE',  ( 8.641460742840918030, -32.93424481021354921, 7.321391277662001151 ) ) ;
#5366 = ORIENTED_EDGE ( 'NONE', *, *, #13357, .T. ) ;
#5367 = EDGE_CURVE ( 'NONE', #1806, #9791, #10603, .T. ) ;
#5368 = ORIENTED_EDGE ( 'NONE', *, *, #9851, .T. ) ;
#5369 = AXIS2_PLACEMENT_3D ( 'NONE', #7438, #13080, #17604 ) ;
#5370 = DIRECTION ( 'NONE',  ( 1.000000000000000000, 0.000000000000000000, 0.000000000000000000 ) ) ;
#5371 = ORIENTED_EDGE ( 'NONE', *, *, #9646, .T. ) ;
#5372 = CYLINDRICAL_SURFACE ( 'NONE', #5698, 0.2999999999999999334 ) ;
#5373 = EDGE_LOOP ( 'NONE', ( #634, #5322, #2855, #9002 ) ) ;
#5374 = ORIENTED_EDGE ( 'NONE', *, *, #2588, .F. ) ;
#5375 = EDGE_CURVE ( 'NONE', #20875, #12990, #18093, .T. ) ;
#5376 = AXIS2_PLACEMENT_3D ( 'NONE', #14924, #16150, #12796 ) ;
#5377 = CIRCLE ( 'NONE', #17859, 4.193574995607837863 ) ;
#5378 = VERTEX_POINT ( 'NONE', #22057 ) ;
#5379 = CARTESIAN_POINT ( 'NONE',  ( 15.21174975910705918, 52.10286008774954780, 13.87500000000000000 ) ) ;
#5380 = AXIS2_PLACEMENT_3D ( 'NONE', #7766, #11212, #19842 ) ;
#5381 = CYLINDRICAL_SURFACE ( 'NONE', #2577, 2.000000000000001776 ) ;
#5382 = EDGE_CURVE ( 'NONE', #2230, #5647, #4524, .T. ) ;
#5383 = PLANE ( 'NONE',  #10311 ) ;
#5384 = ADVANCED_FACE ( 'NONE', ( #3355 ), #16651, .T. ) ;
#5385 = CARTESIAN_POINT ( 'NONE',  ( 29.13662752439705272, -5.000000000000000000, 7.200000000000000178 ) ) ;
#5386 = UNCERTAINTY_MEASURE_WITH_UNIT (LENGTH_MEASURE( 1.000000000000000082E-05 ), #14782, 'distance_accuracy_value', 'NONE');
#5387 = CARTESIAN_POINT ( 'NONE',  ( -30.67540678000428045, -6.000000000000000000, 3.799999999999999822 ) ) ;
#5388 = DIRECTION ( 'NONE',  ( 0.000000000000000000, 0.000000000000000000, 1.000000000000000000 ) ) ;
#5389 = CARTESIAN_POINT ( 'NONE',  ( 30.37540678000427619, -6.000000000000000000, 3.799999999999999822 ) ) ;
#5390 = ORIENTED_EDGE ( 'NONE', *, *, #11702, .T. ) ;
#5391 = LINE ( 'NONE', #5055, #19208 ) ;
#5392 = CYLINDRICAL_SURFACE ( 'NONE', #17751, 0.1000000000000028644 ) ;
#5393 = VECTOR ( 'NONE', #8757, 1000.000000000000000 ) ;
#5394 = VERTEX_POINT ( 'NONE', #10182 ) ;
#5395 = ORIENTED_EDGE ( 'NONE', *, *, #14899, .F. ) ;
#5396 = DIRECTION ( 'NONE',  ( 0.000000000000000000, -1.000000000000000000, 0.000000000000000000 ) ) ;
#5397 = PRODUCT_CONTEXT ( 'NONE', #19880, 'mechanical' ) ;
#5398 = ADVANCED_FACE ( 'NONE', ( #2920 ), #3818, .T. ) ;
#5399 = ORIENTED_EDGE ( 'NONE', *, *, #16031, .T. ) ;
#5400 = FACE_OUTER_BOUND ( 'NONE', #16610, .T. ) ;
#5401 = ORIENTED_EDGE ( 'NONE', *, *, #10452, .T. ) ;
#5402 = ORIENTED_EDGE ( 'NONE', *, *, #16193, .T. ) ;
#5403 = EDGE_CURVE ( 'NONE', #21455, #6635, #13787, .T. ) ;
#5404 = VECTOR ( 'NONE', #563, 1000.000000000000000 ) ;
#5405 = LINE ( 'NONE', #7191, #4868 ) ;
#5406 = EDGE_CURVE ( 'NONE', #3943, #12842, #11955, .T. ) ;
#5407 = LINE ( 'NONE', #10533, #12345 ) ;
#5408 = CARTESIAN_POINT ( 'NONE',  ( 15.95292532278785913, 52.10286008774954780, 13.87499999999999822 ) ) ;
#5409 = AXIS2_PLACEMENT_3D ( 'NONE', #6853, #11523, #5049 ) ;
#5410 = ADVANCED_FACE ( 'NONE', ( #6851 ), #11262, .F. ) ;
#5411 = CARTESIAN_POINT ( 'NONE',  ( 9.641460742840918030, 32.61873716947361856, 68.00000000000000000 ) ) ;
#5412 = CARTESIAN_POINT ( 'NONE',  ( 29.69597781366221767, 56.94165929845684104, 70.50000000000000000 ) ) ;
#5413 = CARTESIAN_POINT ( 'NONE',  ( -23.02398829872513986, 2.157133714763345367, 13.26827027136043213 ) ) ;
#5414 = CARTESIAN_POINT ( 'NONE',  ( 34.69999999999999574, 84.70000000000001705, 3.009745230819759520E-15 ) ) ;
#5415 = DIRECTION ( 'NONE',  ( -0.4461977533474358326, -1.454668808886070861E-15, -0.8949343913984425525 ) ) ;
#5416 = CARTESIAN_POINT ( 'NONE',  ( 0.000000000000000000, -32.61873716947361856, 68.00000000000000000 ) ) ;
#5417 = FACE_OUTER_BOUND ( 'NONE', #17563, .T. ) ;
#5418 = AXIS2_PLACEMENT_3D ( 'NONE', #7124, #18746, #22132 ) ;
#5419 = ORIENTED_EDGE ( 'NONE', *, *, #11402, .F. ) ;
#5420 = EDGE_LOOP ( 'NONE', ( #17716, #21461, #10222, #7016 ) ) ;
#5421 = DIRECTION ( 'NONE',  ( -3.052134192567367925E-16, 1.000000000000000000, -0.000000000000000000 ) ) ;
#5422 = CARTESIAN_POINT ( 'NONE',  ( -30.49999999999998934, 69.70000000000001705, 1.500000000000001332 ) ) ;
#5423 = EDGE_CURVE ( 'NONE', #8790, #1357, #11302, .T. ) ;
#5424 = ORIENTED_EDGE ( 'NONE', *, *, #21476, .T. ) ;
#5425 = CIRCLE ( 'NONE', #16786, 0.5000000000000004441 ) ;
#5426 = VECTOR ( 'NONE', #15906, 1000.000000000000000 ) ;
#5427 = LINE ( 'NONE', #18850, #2021 ) ;
#5428 = ADVANCED_FACE ( 'NONE', ( #16626 ), #13089, .T. ) ;
#5429 = AXIS2_PLACEMENT_3D ( 'NONE', #17250, #8660, #6984 ) ;
#5430 = CARTESIAN_POINT ( 'NONE',  ( 33.79999999999999716, 84.70000000000001705, 1.799999999999996048 ) ) ;
#5431 = AXIS2_PLACEMENT_3D ( 'NONE', #13673, #10219, #17151 ) ;
#5432 = ADVANCED_FACE ( 'NONE', ( #11713 ), #14963, .F. ) ;
#5433 = LINE ( 'NONE', #3737, #567 ) ;
#5434 = VERTEX_POINT ( 'NONE', #1529 ) ;
#5435 = DIRECTION ( 'NONE',  ( -1.000000000000000000, 0.000000000000000000, 0.000000000000000000 ) ) ;
#5436 = ADVANCED_FACE ( 'NONE', ( #8040 ), #16420, .T. ) ;
#5437 = DIRECTION ( 'NONE',  ( 0.000000000000000000, 0.000000000000000000, -1.000000000000000000 ) ) ;
#5438 = DIRECTION ( 'NONE',  ( -6.123233995736764803E-17, 0.000000000000000000, 1.000000000000000000 ) ) ;
#5439 = DIRECTION ( 'NONE',  ( 0.000000000000000000, 0.000000000000000000, 1.000000000000000000 ) ) ;
#5440 = DIRECTION ( 'NONE',  ( 0.000000000000000000, 0.000000000000000000, 1.000000000000000000 ) ) ;
#5441 = DIRECTION ( 'NONE',  ( -1.000000000000000000, 0.000000000000000000, 0.000000000000000000 ) ) ;
#5442 = EDGE_LOOP ( 'NONE', ( #18710, #928, #2547, #9957, #20871, #7879 ) ) ;
#5443 = LINE ( 'NONE', #1314, #6498 ) ;
#5444 = CARTESIAN_POINT ( 'NONE',  ( 29.13662752439705272, 0.000000000000000000, 3.500000000000000000 ) ) ;
#5445 = DIRECTION ( 'NONE',  ( -4.336808689941893885E-15, 0.000000000000000000, 1.000000000000000000 ) ) ;
#5446 = VERTEX_POINT ( 'NONE', #1092 ) ;
#5447 = VECTOR ( 'NONE', #6013, 1000.000000000000000 ) ;
#5448 = ORIENTED_EDGE ( 'NONE', *, *, #16031, .F. ) ;
#5449 = ORIENTED_EDGE ( 'NONE', *, *, #7694, .F. ) ;
#5450 = CYLINDRICAL_SURFACE ( 'NONE', #16336, 0.04999999999999991257 ) ;
#5451 = DIRECTION ( 'NONE',  ( 2.388292521039847891E-16, -0.000000000000000000, 1.000000000000000000 ) ) ;
#5452 = APPLICATION_CONTEXT ( 'automotive_design' ) ;
#5453 = CIRCLE ( 'NONE', #11141, 0.05000000000000143219 ) ;
#5454 = DIRECTION ( 'NONE',  ( 1.000000000000000000, 0.000000000000000000, 0.000000000000000000 ) ) ;
#5455 = EDGE_CURVE ( 'NONE', #11459, #3680, #19906, .T. ) ;
#5456 = AXIS2_PLACEMENT_3D ( 'NONE', #12888, #4181, #17934 ) ;
#5457 = AXIS2_PLACEMENT_3D ( 'NONE', #19347, #21150, #11056 ) ;
#5458 = AXIS2_PLACEMENT_3D ( 'NONE', #9511, #7961, #7851 ) ;
#5459 = DIRECTION ( 'NONE',  ( 0.000000000000000000, -1.000000000000000000, 0.000000000000000000 ) ) ;
#5460 = ADVANCED_FACE ( 'NONE', ( #21811 ), #4567, .T. ) ;
#5461 = ORIENTED_EDGE ( 'NONE', *, *, #12546, .T. ) ;
#5462 = DIRECTION ( 'NONE',  ( 1.000000000000000000, 0.000000000000000000, -0.000000000000000000 ) ) ;
#5463 = VERTEX_POINT ( 'NONE', #14841 ) ;
#5464 = DIRECTION ( 'NONE',  ( 0.000000000000000000, 0.000000000000000000, 1.000000000000000000 ) ) ;
#5465 = CARTESIAN_POINT ( 'NONE',  ( 0.000000000000000000, -5.299999999999999822, 7.500000000000000000 ) ) ;
#5466 = DIRECTION ( 'NONE',  ( 0.000000000000000000, 0.000000000000000000, -1.000000000000000000 ) ) ;
#5467 = CARTESIAN_POINT ( 'NONE',  ( -1.824728116533986810, 42.36054587065083155, 53.71679706732590631 ) ) ;
#5468 = VERTEX_POINT ( 'NONE', #6489 ) ;
#5469 = DIRECTION ( 'NONE',  ( 0.000000000000000000, 0.000000000000000000, -1.000000000000000000 ) ) ;
#5470 = ADVANCED_FACE ( 'NONE', ( #13386 ), #5962, .T. ) ;
#5471 = CARTESIAN_POINT ( 'NONE',  ( -33.20000000000001705, 85.00000000000000000, 78.79999999999999716 ) ) ;
#5472 = CIRCLE ( 'NONE', #14011, 4.575000000000001066 ) ;
#5473 = DIRECTION ( 'NONE',  ( -0.000000000000000000, -1.000000000000000000, -0.000000000000000000 ) ) ;
#5474 = PLANE ( 'NONE',  #8889 ) ;
#5475 = VERTEX_POINT ( 'NONE', #4788 ) ;
#5476 = CARTESIAN_POINT ( 'NONE',  ( 0.000000000000000000, 0.000000000000000000, 68.50000000000000000 ) ) ;
#5477 = ORIENTED_EDGE ( 'NONE', *, *, #12770, .F. ) ;
#5478 = CARTESIAN_POINT ( 'NONE',  ( 1.724728116533979838, 43.31054587065082728, 49.66679706732590915 ) ) ;
#5479 = CARTESIAN_POINT ( 'NONE',  ( -17.95292532278785913, 0.000000000000000000, 42.50000000000000711 ) ) ;
#5480 = ORIENTED_EDGE ( 'NONE', *, *, #12572, .F. ) ;
#5481 = ORIENTED_EDGE ( 'NONE', *, *, #1445, .F. ) ;
#5482 = CIRCLE ( 'NONE', #14019, 0.2999999999999999334 ) ;
#5483 = PLANE ( 'NONE',  #6056 ) ;
#5484 = DIRECTION ( 'NONE',  ( 0.000000000000000000, 0.000000000000000000, 1.000000000000000000 ) ) ;
#5485 = VERTEX_POINT ( 'NONE', #19902 ) ;
#5486 = ORIENTED_EDGE ( 'NONE', *, *, #20977, .T. ) ;
#5487 = EDGE_CURVE ( 'NONE', #17759, #14667, #8819, .T. ) ;
#5488 = EDGE_CURVE ( 'NONE', #9687, #20783, #8464, .T. ) ;
#5489 = ORIENTED_EDGE ( 'NONE', *, *, #20815, .F. ) ;
#5490 = ADVANCED_FACE ( 'NONE', ( #3103 ), #12709, .T. ) ;
#5491 = ORIENTED_EDGE ( 'NONE', *, *, #14973, .F. ) ;
#5492 = DIRECTION ( 'NONE',  ( 0.000000000000000000, 0.000000000000000000, 1.000000000000000000 ) ) ;
#5493 = DIRECTION ( 'NONE',  ( 0.000000000000000000, 1.000000000000000000, 0.000000000000000000 ) ) ;
#5494 = DIRECTION ( 'NONE',  ( 1.000000000000000000, 0.000000000000000000, 0.000000000000000000 ) ) ;
#5495 = FACE_OUTER_BOUND ( 'NONE', #10139, .T. ) ;
#5496 = DIRECTION ( 'NONE',  ( -0.000000000000000000, -1.000000000000000000, -0.000000000000000000 ) ) ;
#5497 = ORIENTED_EDGE ( 'NONE', *, *, #733, .F. ) ;
#5498 = CARTESIAN_POINT ( 'NONE',  ( -17.95292532278785913, 34.11873716947361856, 109.6002446535588319 ) ) ;
#5499 = DIRECTION ( 'NONE',  ( -0.000000000000000000, -0.000000000000000000, -1.000000000000000000 ) ) ;
#5500 = DIRECTION ( 'NONE',  ( 1.000000000000000000, 0.000000000000000000, 0.000000000000000000 ) ) ;
#5501 = PRODUCT_RELATED_PRODUCT_CATEGORY ( 'part', '', ( #1228 ) ) ;
#5502 = VERTEX_POINT ( 'NONE', #8262 ) ;
#5503 = CARTESIAN_POINT ( 'NONE',  ( -1.774728116533986766, 43.31054587065082728, 45.66679706732590205 ) ) ;
#5504 = CARTESIAN_POINT ( 'NONE',  ( -14.98564789012718101, 51.95085597973990588, 13.85527924978055481 ) ) ;
#5505 = ORIENTED_EDGE ( 'NONE', *, *, #2256, .T. ) ;
#5506 = ORIENTED_EDGE ( 'NONE', *, *, #211, .T. ) ;
#5507 = ORIENTED_EDGE ( 'NONE', *, *, #5662, .T. ) ;
#5508 = CARTESIAN_POINT ( 'NONE',  ( -4.127054932750482408, 33.93424481021354921, 68.00000000000000000 ) ) ;
#5509 = ADVANCED_FACE ( 'NONE', ( #4684 ), #17746, .T. ) ;
#5510 = ORIENTED_EDGE ( 'NONE', *, *, #15368, .T. ) ;
#5511 =( GEOMETRIC_REPRESENTATION_CONTEXT ( 3 ) GLOBAL_UNCERTAINTY_ASSIGNED_CONTEXT ( ( #19027 ) ) GLOBAL_UNIT_ASSIGNED_CONTEXT ( ( #3960, #7540, #14340 ) ) REPRESENTATION_CONTEXT ( 'NONE', 'WORKASPACE' ) );
#5512 = LINE ( 'NONE', #12290, #19021 ) ;
#5513 = ORIENTED_EDGE ( 'NONE', *, *, #8974, .T. ) ;
#5514 = ORIENTED_EDGE ( 'NONE', *, *, #6871, .F. ) ;
#5515 = DIRECTION ( 'NONE',  ( 0.000000000000000000, 0.000000000000000000, -1.000000000000000000 ) ) ;
#5516 = AXIS2_PLACEMENT_3D ( 'NONE', #18894, #13718, #10159 ) ;
#5517 = SURFACE_SIDE_STYLE ('',( #10905 ) ) ;
#5518 = CARTESIAN_POINT ( 'NONE',  ( -29.37540678000427619, 6.000000000000000000, 3.799999999999999822 ) ) ;
#5519 = CARTESIAN_POINT ( 'NONE',  ( 28.64417692495746692, 6.713479613976641502, 13.50000000000000000 ) ) ;
#5520 = TOROIDAL_SURFACE ( 'NONE', #8369, 0.2999999999999999889, 0.2999999999999999889 ) ;
#5521 = CARTESIAN_POINT ( 'NONE',  ( -29.37540678000427619, 5.000000000000000000, 7.200000000000000178 ) ) ;
#5522 = CARTESIAN_POINT ( 'NONE',  ( -1.724728116533986721, 43.31054587065082728, 41.76679706732590347 ) ) ;
#5523 = CARTESIAN_POINT ( 'NONE',  ( 14.96174975910707161, -51.86873716947361856, 68.00000000000000000 ) ) ;
#5524 = TOROIDAL_SURFACE ( 'NONE', #5167, 0.7000000000000000666, 0.2999999999999999889 ) ;
#5525 = CARTESIAN_POINT ( 'NONE',  ( 29.13662752439705272, 0.000000000000000000, 7.200000000000000178 ) ) ;
#5526 = CARTESIAN_POINT ( 'NONE',  ( -25.37540678000427263, -67.24634676501045760, 13.19999999999999929 ) ) ;
#5527 = ORIENTED_EDGE ( 'NONE', *, *, #14572, .F. ) ;
#5528 = VERTEX_POINT ( 'NONE', #21918 ) ;
#5529 = CARTESIAN_POINT ( 'NONE',  ( -29.37540678000427619, 6.000000000000000000, 7.200000000000000178 ) ) ;
#5530 = EDGE_CURVE ( 'NONE', #18467, #18812, #3223, .T. ) ;
#5531 = CARTESIAN_POINT ( 'NONE',  ( 26.56227312273159313, -9.958410664601842655, 42.50000000000000000 ) ) ;
#5532 = EDGE_CURVE ( 'NONE', #13239, #2467, #21484, .T. ) ;
#5533 = VERTEX_POINT ( 'NONE', #17383 ) ;
#5534 = VERTEX_POINT ( 'NONE', #17503 ) ;
#5535 = ADVANCED_FACE ( 'NONE', ( #20869 ), #19078, .T. ) ;
#5536 = CYLINDRICAL_SURFACE ( 'NONE', #15312, 0.2999999999999999334 ) ;
#5537 = DIRECTION ( 'NONE',  ( 1.000000000000000000, 0.000000000000000000, 0.000000000000000000 ) ) ;
#5538 = ORIENTED_EDGE ( 'NONE', *, *, #6225, .F. ) ;
#5539 = CARTESIAN_POINT ( 'NONE',  ( 23.32398829872514057, -2.157133568460767759, 13.19999999999999929 ) ) ;
#5540 = FACE_OUTER_BOUND ( 'NONE', #17260, .T. ) ;
#5541 = EDGE_CURVE ( 'NONE', #15844, #12670, #10688, .T. ) ;
#5542 = CARTESIAN_POINT ( 'NONE',  ( -1.824728116533986810, 42.36054587065083155, 35.70876104995653577 ) ) ;
#5543 = LINE ( 'NONE', #8684, #10873 ) ;
#5544 = CARTESIAN_POINT ( 'NONE',  ( 0.000000000000000000, 43.26054587065083012, 53.71679706732590631 ) ) ;
#5545 = DIRECTION ( 'NONE',  ( -0.000000000000000000, 1.000000000000000000, -0.000000000000000000 ) ) ;
#5546 = DIRECTION ( 'NONE',  ( -0.000000000000000000, 0.000000000000000000, -1.000000000000000000 ) ) ;
#5547 = LINE ( 'NONE', #3869, #8273 ) ;
#5548 = DIRECTION ( 'NONE',  ( 1.000000000000000000, 0.000000000000000000, 0.000000000000000000 ) ) ;
#5549 = DIRECTION ( 'NONE',  ( 0.000000000000000000, 1.000000000000000000, -0.000000000000000000 ) ) ;
#5550 = VERTEX_POINT ( 'NONE', #2169 ) ;
#5551 = AXIS2_PLACEMENT_3D ( 'NONE', #13423, #21737, #18350 ) ;
#5552 = VERTEX_POINT ( 'NONE', #5669 ) ;
#5553 = AXIS2_PLACEMENT_3D ( 'NONE', #21188, #12973, #19480 ) ;
#5554 = ORIENTED_EDGE ( 'NONE', *, *, #13761, .F. ) ;
#5555 = DIRECTION ( 'NONE',  ( 0.000000000000000000, 0.000000000000000000, -1.000000000000000000 ) ) ;
#5556 = CARTESIAN_POINT ( 'NONE',  ( -18.22752199202934520, 38.74634676501045760, 13.79999999999999893 ) ) ;
#5557 = EDGE_CURVE ( 'NONE', #9928, #20941, #9418, .T. ) ;
#5558 = DIRECTION ( 'NONE',  ( 1.000000000000000000, -0.000000000000000000, 0.000000000000000000 ) ) ;
#5559 = EDGE_CURVE ( 'NONE', #6504, #398, #20624, .T. ) ;
#5560 = EDGE_LOOP ( 'NONE', ( #19728, #2017, #7315, #14694 ) ) ;
#5561 = ADVANCED_FACE ( 'NONE', ( #6801 ), #1397, .T. ) ;
#5562 = DIRECTION ( 'NONE',  ( -0.2309407893632008379, 0.9729678061520339316, -0.000000000000000000 ) ) ;
#5563 = EDGE_CURVE ( 'NONE', #6583, #11049, #10959, .T. ) ;
#5564 = ORIENTED_EDGE ( 'NONE', *, *, #13912, .F. ) ;
#5565 = DIRECTION ( 'NONE',  ( 0.000000000000000000, 0.000000000000000000, 1.000000000000000000 ) ) ;
#5566 = EDGE_LOOP ( 'NONE', ( #14554, #9681, #14712, #21295 ) ) ;
#5567 = CARTESIAN_POINT ( 'NONE',  ( -11.70301280599631433, -2.777792850139019443, 13.74999999999999822 ) ) ;
#5568 = DIRECTION ( 'NONE',  ( -0.000000000000000000, -1.000000000000000000, -0.000000000000000000 ) ) ;
#5569 = DIRECTION ( 'NONE',  ( 1.000000000000000000, 0.000000000000000000, 0.000000000000000000 ) ) ;
#5570 = AXIS2_PLACEMENT_3D ( 'NONE', #12364, #15619, #13947 ) ;
#5571 = CARTESIAN_POINT ( 'NONE',  ( -15.21174975910705207, -42.11054587065083155, 13.50000000000000000 ) ) ;
#5572 = ORIENTED_EDGE ( 'NONE', *, *, #517, .T. ) ;
#5573 = DIRECTION ( 'NONE',  ( 1.000000000000000000, 0.000000000000000000, -2.107255972850002284E-16 ) ) ;
#5574 = CARTESIAN_POINT ( 'NONE',  ( 0.000000000000000000, 0.000000000000000000, 13.50000000000000000 ) ) ;
#5575 = ADVANCED_FACE ( 'NONE', ( #13656 ), #4845, .T. ) ;
#5576 = DIRECTION ( 'NONE',  ( -2.388292521039847891E-16, 0.000000000000000000, -1.000000000000000000 ) ) ;
#5577 = FACE_OUTER_BOUND ( 'NONE', #4972, .T. ) ;
#5578 = ORIENTED_EDGE ( 'NONE', *, *, #16295, .T. ) ;
#5579 = SURFACE_SIDE_STYLE ('',( #8818 ) ) ;
#5580 = ORIENTED_EDGE ( 'NONE', *, *, #1035, .T. ) ;
#5581 = DIRECTION ( 'NONE',  ( -0.000000000000000000, -0.000000000000000000, -1.000000000000000000 ) ) ;
#5582 = DIRECTION ( 'NONE',  ( 0.000000000000000000, 1.000000000000000000, -0.000000000000000000 ) ) ;
#5583 = ORIENTED_EDGE ( 'NONE', *, *, #3776, .T. ) ;
#5584 = TOROIDAL_SURFACE ( 'NONE', #2332, 0.5999999999999999778, 0.2999999999999999889 ) ;
#5585 = VERTEX_POINT ( 'NONE', #1803 ) ;
#5586 = DIRECTION ( 'NONE',  ( 1.000000000000000000, -0.000000000000000000, -0.000000000000000000 ) ) ;
#5587 = EDGE_CURVE ( 'NONE', #18470, #6298, #13414, .T. ) ;
#5588 = AXIS2_PLACEMENT_3D ( 'NONE', #10761, #15550, #19149 ) ;
#5589 = ORIENTED_EDGE ( 'NONE', *, *, #10349, .F. ) ;
#5590 = CIRCLE ( 'NONE', #18784, 1.499999999999999556 ) ;
#5591 = EDGE_CURVE ( 'NONE', #19345, #16058, #17233, .T. ) ;
#5592 = ORIENTED_EDGE ( 'NONE', *, *, #19954, .F. ) ;
#5593 = EDGE_LOOP ( 'NONE', ( #15520, #11531, #7924, #14947 ) ) ;
#5594 = CYLINDRICAL_SURFACE ( 'NONE', #2055, 0.3000000000000003775 ) ;
#5595 = AXIS2_PLACEMENT_3D ( 'NONE', #8712, #10490, #17298 ) ;
#5596 = VECTOR ( 'NONE', #8227, 1000.000000000000000 ) ;
#5597 = DIRECTION ( 'NONE',  ( 0.000000000000000000, 0.000000000000000000, -1.000000000000000000 ) ) ;
#5598 = TOROIDAL_SURFACE ( 'NONE', #5945, 0.7000000000000000666, 0.2999999999999999889 ) ;
#5599 = DIRECTION ( 'NONE',  ( -1.000000000000000000, 0.000000000000000000, 0.000000000000000000 ) ) ;
#5600 = DIRECTION ( 'NONE',  ( -0.000000000000000000, -0.000000000000000000, -1.000000000000000000 ) ) ;
#5601 = CARTESIAN_POINT ( 'NONE',  ( 25.37540678000427263, 63.74634676501045050, 7.500000000000000000 ) ) ;
#5602 = VERTEX_POINT ( 'NONE', #6863 ) ;
#5603 = CARTESIAN_POINT ( 'NONE',  ( -18.22752199202934520, 39.04634676501046187, 13.50000000000000000 ) ) ;
#5604 = VECTOR ( 'NONE', #8774, 1000.000000000000000 ) ;
#5605 = EDGE_CURVE ( 'NONE', #2324, #19220, #15448, .T. ) ;
#5606 = DIRECTION ( 'NONE',  ( 0.000000000000000000, 0.000000000000000000, 1.000000000000000000 ) ) ;
#5607 = ADVANCED_FACE ( 'NONE', ( #17121 ), #5584, .T. ) ;
#5608 = DIRECTION ( 'NONE',  ( 0.000000000000000000, 0.000000000000000000, 1.000000000000000000 ) ) ;
#5609 = B_SPLINE_CURVE_WITH_KNOTS ( 'NONE', 3,
 ( #5775, #4299, #19186, #5877, #8901, #2504, #14356, #14453 ),
 .UNSPECIFIED., .F., .F.,
 ( 4, 2, 2, 4 ),
 ( -3.470042892451968281E-06, 0.0002769752510348927397, 0.0004171978979985645165, 0.0005574205449622362391 ),
 .UNSPECIFIED. ) ;
#5610 = ORIENTED_EDGE ( 'NONE', *, *, #11700, .F. ) ;
#5611 = CARTESIAN_POINT ( 'NONE',  ( 1.774728116533973665, 42.31054587065082728, 20.00000000000000000 ) ) ;
#5612 = ORIENTED_EDGE ( 'NONE', *, *, #6604, .F. ) ;
#5613 = CIRCLE ( 'NONE', #11298, 0.5000000000000004441 ) ;
#5614 = CIRCLE ( 'NONE', #214, 4.999999999999997335 ) ;
#5615 = ORIENTED_EDGE ( 'NONE', *, *, #9770, .T. ) ;
#5616 = AXIS2_PLACEMENT_3D ( 'NONE', #21276, #12739, #7527 ) ;
#5617 = CARTESIAN_POINT ( 'NONE',  ( -31.50000000000002132, 71.70000000000001705, 3.500000000000000000 ) ) ;
#5619 = EDGE_CURVE ( 'NONE', #1813, #17313, #107, .T. ) ;
#5618 = ITEM_DEFINED_TRANSFORMATION ( 'NONE', 'NONE', #16188,  #17493 ) ;
#5620 = ORIENTED_EDGE ( 'NONE', *, *, #9724, .T. ) ;
#5621 = ORIENTED_EDGE ( 'NONE', *, *, #16575, .F. ) ;
#5622 = CIRCLE ( 'NONE', #12716, 0.04999999999999991257 ) ;
#5623 = CARTESIAN_POINT ( 'NONE',  ( -26.33662752439704846, 0.000000000000000000, 8.402566836762659364E-16 ) ) ;
#5624 = ORIENTED_EDGE ( 'NONE', *, *, #7761, .T. ) ;
#5625 = ORIENTED_EDGE ( 'NONE', *, *, #14674, .F. ) ;
#5626 = CARTESIAN_POINT ( 'NONE',  ( 1.724728116533979616, 43.31054587065082728, 27.80876104995653719 ) ) ;
#5627 = CARTESIAN_POINT ( 'NONE',  ( -30.79999999999999005, 69.70000000000001705, 1.500000000000000222 ) ) ;
#5628 = PRESENTATION_STYLE_ASSIGNMENT (( #9079 ) ) ;
#5629 = LINE ( 'NONE', #12418, #10578 ) ;
#5630 = VECTOR ( 'NONE', #15693, 1000.000000000000000 ) ;
#5631 = AXIS2_PLACEMENT_3D ( 'NONE', #18452, #3134, #16774 ) ;
#5632 = CIRCLE ( 'NONE', #1323, 0.05000000000000143219 ) ;
#5633 = DIRECTION ( 'NONE',  ( -1.000000000000000000, -2.105859220307275826E-16, 0.000000000000000000 ) ) ;
#5634 = EDGE_CURVE ( 'NONE', #15404, #22008, #14994, .T. ) ;
#5635 = AXIS2_PLACEMENT_3D ( 'NONE', #8951, #7061, #13855 ) ;
#5636 = CARTESIAN_POINT ( 'NONE',  ( -23.07499583180669234, 2.433548416302913520, 13.33575415462846081 ) ) ;
#5637 = CIRCLE ( 'NONE', #7417, 0.05000000000000143219 ) ;
#5638 = DIRECTION ( 'NONE',  ( 8.673617379884034239E-17, 0.000000000000000000, -1.000000000000000000 ) ) ;
#5639 = EDGE_CURVE ( 'NONE', #1886, #9580, #8291, .T. ) ;
#5640 = CARTESIAN_POINT ( 'NONE',  ( -1.724728116533986721, 43.31054587065082728, 27.80876104995653719 ) ) ;
#5641 = TOROIDAL_SURFACE ( 'NONE', #14527, 2.274596669241483848, 0.2999999999999999889 ) ;
#5642 = CARTESIAN_POINT ( 'NONE',  ( -14.96244602927844980, -51.84405746083547939, 13.82646097708239452 ) ) ;
#5643 = VERTEX_POINT ( 'NONE', #18117 ) ;
#5644 = ORIENTED_EDGE ( 'NONE', *, *, #12702, .F. ) ;
#5645 = CARTESIAN_POINT ( 'NONE',  ( 23.02398829872513986, 7.027230193580998154E-15, 13.79999999999999893 ) ) ;
#5646 = DIRECTION ( 'NONE',  ( -1.000000000000000000, 0.000000000000000000, 0.000000000000000000 ) ) ;
#5647 = VERTEX_POINT ( 'NONE', #18648 ) ;
#5648 = ORIENTED_EDGE ( 'NONE', *, *, #8192, .F. ) ;
#5649 = VECTOR ( 'NONE', #14960, 1000.000000000000000 ) ;
#5650 = CIRCLE ( 'NONE', #17064, 0.05000000000000143219 ) ;
#5651 = ORIENTED_EDGE ( 'NONE', *, *, #3129, .T. ) ;
#5652 = VECTOR ( 'NONE', #11018, 1000.000000000000000 ) ;
#5653 = B_SPLINE_CURVE_WITH_KNOTS ( 'NONE', 3,
 ( #9694, #4531, #18392, #17954, #19991, #829, #16594, #6339, #13251, #2627 ),
 .UNSPECIFIED., .F., .F.,
 ( 4, 2, 2, 2, 4 ),
 ( 0.000000000000000000, 0.0007882085451459004124, 0.001182312817718851215, 0.001379364954005326670, 0.001576417090291802126 ),
 .UNSPECIFIED. ) ;
#5654 = EDGE_CURVE ( 'NONE', #20520, #16071, #10218, .T. ) ;
#5655 = CIRCLE ( 'NONE', #3149, 0.05000000000000143219 ) ;
#5656 = PLANE ( 'NONE',  #16368 ) ;
#5657 = DIRECTION ( 'NONE',  ( 0.000000000000000000, -1.000000000000000000, 0.000000000000000000 ) ) ;
#5658 = ORIENTED_EDGE ( 'NONE', *, *, #1386, .F. ) ;
#5659 = DIRECTION ( 'NONE',  ( 1.000000000000000000, 0.000000000000000000, 0.000000000000000000 ) ) ;
#5660 = CARTESIAN_POINT ( 'NONE',  ( -1.724728116533986721, 43.26054587065083012, 31.70876104995653932 ) ) ;
#5661 = EDGE_CURVE ( 'NONE', #19800, #1806, #3782, .T. ) ;
#5662 = EDGE_CURVE ( 'NONE', #5035, #18477, #9509, .T. ) ;
#5663 = DIRECTION ( 'NONE',  ( 0.000000000000000000, 0.000000000000000000, 1.000000000000000000 ) ) ;
#5664 = LINE ( 'NONE', #15485, #3369 ) ;
#5665 = DIRECTION ( 'NONE',  ( -1.000000000000000000, 0.000000000000000000, 0.000000000000000000 ) ) ;
#5666 = AXIS2_PLACEMENT_3D ( 'NONE', #636, #10611, #19440 ) ;
#5667 = DIRECTION ( 'NONE',  ( 1.000000000000000000, -0.000000000000000000, 1.734723475976806848E-16 ) ) ;
#5668 = MANIFOLD_SOLID_BREP ( 'Stock-MAS-696-1', #20640 ) ;
#5669 = CARTESIAN_POINT ( 'NONE',  ( -31.26086011588028057, 83.95073979834610611, 13.50000000000000000 ) ) ;
#5670 = DIRECTION ( 'NONE',  ( 0.000000000000000000, 0.000000000000000000, 1.000000000000000000 ) ) ;
#5671 = DIRECTION ( 'NONE',  ( 0.000000000000000000, 0.000000000000000000, 1.000000000000000000 ) ) ;
#5672 = CIRCLE ( 'NONE', #21752, 0.05000000000000143219 ) ;
#5673 = DIRECTION ( 'NONE',  ( -1.000000000000000000, 3.009265538104883829E-28, -4.336808689941893885E-15 ) ) ;
#5674 = EDGE_LOOP ( 'NONE', ( #13232, #5345, #6578, #4147 ) ) ;
#5675 = ORIENTED_EDGE ( 'NONE', *, *, #7343, .F. ) ;
#5676 = VECTOR ( 'NONE', #19487, 1000.000000000000000 ) ;
#5677 = ORIENTED_EDGE ( 'NONE', *, *, #19603, .F. ) ;
#5678 = CYLINDRICAL_SURFACE ( 'NONE', #15278, 0.2999999999999999889 ) ;
#5679 = VECTOR ( 'NONE', #15296, 1000.000000000000000 ) ;
#5680 = DIRECTION ( 'NONE',  ( -1.000000000000000000, 0.000000000000000000, 0.000000000000000000 ) ) ;
#5681 = ORIENTED_EDGE ( 'NONE', *, *, #9324, .F. ) ;
#5682 = CARTESIAN_POINT ( 'NONE',  ( -1.724728116533986721, 43.26054587065083012, 45.66679706732590205 ) ) ;
#5683 = ADVANCED_FACE ( 'NONE', ( #3947 ), #10763, .F. ) ;
#5684 = VERTEX_POINT ( 'NONE', #7193 ) ;
#5685 = DIRECTION ( 'NONE',  ( 0.000000000000000000, 0.000000000000000000, 1.000000000000000000 ) ) ;
#5686 = CIRCLE ( 'NONE', #17757, 0.2500000000000002220 ) ;
#5687 = VECTOR ( 'NONE', #14732, 1000.000000000000000 ) ;
#5688 = CARTESIAN_POINT ( 'NONE',  ( -29.13662752439705272, 0.000000000000000000, 3.500000000000000000 ) ) ;
#5689 = ORIENTED_EDGE ( 'NONE', *, *, #10623, .F. ) ;
#5690 = CYLINDRICAL_SURFACE ( 'NONE', #13140, 0.1000000000000028644 ) ;
#5691 = CARTESIAN_POINT ( 'NONE',  ( -9.718906393579157310, 44.91645089659918710, 70.88527860057354246 ) ) ;
#5692 = AXIS2_PLACEMENT_3D ( 'NONE', #17630, #17530, #9033 ) ;
#5693 = LINE ( 'NONE', #17733, #1853 ) ;
#5694 = TOROIDAL_SURFACE ( 'NONE', #10672, 3.200000000000003286, 0.2999999999999999889 ) ;
#5695 = DIRECTION ( 'NONE',  ( -1.000000000000000000, -0.000000000000000000, 0.000000000000000000 ) ) ;
#5696 = ORIENTED_EDGE ( 'NONE', *, *, #2727, .F. ) ;
#5697 = DIRECTION ( 'NONE',  ( 0.000000000000000000, 0.000000000000000000, -1.000000000000000000 ) ) ;
#5698 = AXIS2_PLACEMENT_3D ( 'NONE', #3682, #7491, #8825 ) ;
#5699 = CARTESIAN_POINT ( 'NONE',  ( -1.774728116533986766, 42.31054587065082728, 37.66679706732590915 ) ) ;
#5700 = EDGE_CURVE ( 'NONE', #21031, #11899, #547, .T. ) ;
#5701 = EDGE_CURVE ( 'NONE', #2319, #10473, #12318, .T. ) ;
#5702 = CARTESIAN_POINT ( 'NONE',  ( 1.724728116533979616, 43.26054587065083012, 47.80876104995653719 ) ) ;
#5703 = CARTESIAN_POINT ( 'NONE',  ( -23.21374285137841298, -3.085791193308922153, 13.47995019114138238 ) ) ;
#5704 = EDGE_LOOP ( 'NONE', ( #20829, #5112, #21269, #13676 ) ) ;
#5705 = CARTESIAN_POINT ( 'NONE',  ( -29.37540678000427619, 5.299999999999999822, 7.200000000000000178 ) ) ;
#5706 = ORIENTED_EDGE ( 'NONE', *, *, #12217, .F. ) ;
#5707 = FACE_OUTER_BOUND ( 'NONE', #15341, .T. ) ;
#5708 = DIRECTION ( 'NONE',  ( 0.000000000000000000, 0.000000000000000000, -1.000000000000000000 ) ) ;
#5709 = AXIS2_PLACEMENT_3D ( 'NONE', #11934, #18663, #13719 ) ;
#5710 = ORIENTED_EDGE ( 'NONE', *, *, #12013, .T. ) ;
#5711 = ORIENTED_EDGE ( 'NONE', *, *, #7049, .F. ) ;
#5712 = CARTESIAN_POINT ( 'NONE',  ( 1.824728116533979705, 42.36054587065083155, 29.66679706732590560 ) ) ;
#5713 = DIRECTION ( 'NONE',  ( 0.000000000000000000, 0.000000000000000000, 1.000000000000000000 ) ) ;
#5714 = CIRCLE ( 'NONE', #1757, 0.2999999999999999334 ) ;
#5715 = ORIENTED_EDGE ( 'NONE', *, *, #12616, .F. ) ;
#5716 = CIRCLE ( 'NONE', #8557, 6.499999999999999112 ) ;
#5717 = EDGE_CURVE ( 'NONE', #8125, #11228, #20935, .T. ) ;
#5718 = ORIENTED_EDGE ( 'NONE', *, *, #9309, .F. ) ;
#5719 = CARTESIAN_POINT ( 'NONE',  ( -1.724728116533986721, 43.31054587065082728, 39.75876104995654003 ) ) ;
#5720 = CARTESIAN_POINT ( 'NONE',  ( 14.96174975910705918, -51.76873716947361714, 13.79999999999999716 ) ) ;
#5721 = DIRECTION ( 'NONE',  ( -0.2309407893632113573, 0.9729678061520313781, 0.000000000000000000 ) ) ;
#5722 = DIRECTION ( 'NONE',  ( 0.000000000000000000, 0.000000000000000000, -1.000000000000000000 ) ) ;
#5723 = EDGE_CURVE ( 'NONE', #17419, #16789, #19143, .T. ) ;
#5724 = CIRCLE ( 'NONE', #16041, 0.5000000000000000000 ) ;
#5725 = ADVANCED_FACE ( 'NONE', ( #9490 ), #11271, .T. ) ;
#5726 = VERTEX_POINT ( 'NONE', #17880 ) ;
#5727 = CARTESIAN_POINT ( 'NONE',  ( 1.774728116533979438, 43.31054587065082728, 43.80876104995653719 ) ) ;
#5728 = EDGE_CURVE ( 'NONE', #20699, #13326, #14511, .T. ) ;
#5729 = DIRECTION ( 'NONE',  ( -1.000000000000000000, 0.000000000000000000, 0.000000000000000000 ) ) ;
#5730 = DIRECTION ( 'NONE',  ( -1.000000000000000000, -0.000000000000000000, 0.000000000000000000 ) ) ;
#5731 = EDGE_LOOP ( 'NONE', ( #18643, #13729, #5119, #9922 ) ) ;
#5732 = DIRECTION ( 'NONE',  ( -1.000000000000000000, 0.000000000000000000, 0.000000000000000000 ) ) ;
#5733 = ORIENTED_EDGE ( 'NONE', *, *, #20585, .T. ) ;
#5734 = TOROIDAL_SURFACE ( 'NONE', #4999, 0.05000000000000000278, 0.05000000000000000278 ) ;
#5735 = ORIENTED_EDGE ( 'NONE', *, *, #17881, .T. ) ;
#5736 = CARTESIAN_POINT ( 'NONE',  ( -30.19999999999999574, 70.29999999999999716, 2.939152317953652529E-16 ) ) ;
#5737 = ITEM_DEFINED_TRANSFORMATION ( 'NONE', 'NONE', #13338,  #17493 ) ;
#5738 = AXIS2_PLACEMENT_3D ( 'NONE', #2447, #10940, #2657 ) ;
#5739 = ORIENTED_EDGE ( 'NONE', *, *, #11947, .T. ) ;
#5740 = COLOUR_RGB ( '', 0.08235294, 0.09019608, 0.10196078) ;
#5741 = VECTOR ( 'NONE', #6481, 1000.000000000000000 ) ;
#5742 = ORIENTED_EDGE ( 'NONE', *, *, #16209, .T. ) ;
#5743 = ADVANCED_FACE ( 'NONE', ( #982 ), #4357, .T. ) ;
#5744 = CARTESIAN_POINT ( 'NONE',  ( 23.10703542945396549, -2.595685412882492660, 13.38944394804412852 ) ) ;
#5745 = VERTEX_POINT ( 'NONE', #4247 ) ;
#5746 = DIRECTION ( 'NONE',  ( 0.2309407893632117181, -0.9729678061520313781, -0.000000000000000000 ) ) ;
#5747 = DIRECTION ( 'NONE',  ( 0.000000000000000000, 0.000000000000000000, 1.000000000000000000 ) ) ;
#5748 = CARTESIAN_POINT ( 'NONE',  ( 15.21174975910705918, -41.81054587065082728, 13.75000000000000000 ) ) ;
#5749 = DIRECTION ( 'NONE',  ( 1.000000000000000000, 0.000000000000000000, 0.000000000000000000 ) ) ;
#5750 = EDGE_CURVE ( 'NONE', #712, #2722, #6052, .T. ) ;
#5751 = AXIS2_PLACEMENT_3D ( 'NONE', #5093, #18733, #6664 ) ;
#5752 = AXIS2_PLACEMENT_3D ( 'NONE', #22090, #6550, #18603 ) ;
#5753 = LINE ( 'NONE', #12531, #20119 ) ;
#5754 = CARTESIAN_POINT ( 'NONE',  ( -1.774728116533986766, 43.31054587065082728, 53.66679706732590915 ) ) ;
#5755 = CARTESIAN_POINT ( 'NONE',  ( 14.96174975910707161, -41.81054587065082728, 68.25000000000000000 ) ) ;
#5756 = LINE ( 'NONE', #12534, #20050 ) ;
#5757 = ORIENTED_EDGE ( 'NONE', *, *, #22003, .T. ) ;
#5758 = EDGE_LOOP ( 'NONE', ( #783, #12367, #1973, #18256 ) ) ;
#5759 = DIRECTION ( 'NONE',  ( 0.000000000000000000, 0.000000000000000000, 1.000000000000000000 ) ) ;
#5760 = ORIENTED_EDGE ( 'NONE', *, *, #12240, .F. ) ;
#5761 = ORIENTED_EDGE ( 'NONE', *, *, #8616, .F. ) ;
#5762 = TOROIDAL_SURFACE ( 'NONE', #3610, 0.5999999999999999778, 0.2999999999999999889 ) ;
#5763 = EDGE_CURVE ( 'NONE', #7158, #11635, #15197, .T. ) ;
#5764 = VECTOR ( 'NONE', #6647, 1000.000000000000000 ) ;
#5765 = EDGE_CURVE ( 'NONE', #12192, #1070, #4575, .T. ) ;
#5766 = DIRECTION ( 'NONE',  ( 1.000000000000000000, 0.000000000000000000, 0.000000000000000000 ) ) ;
#5767 = DIRECTION ( 'NONE',  ( 0.000000000000000000, 0.000000000000000000, 1.000000000000000000 ) ) ;
#5768 = ORIENTED_EDGE ( 'NONE', *, *, #1887, .T. ) ;
#5769 = DIRECTION ( 'NONE',  ( 1.000000000000000000, 0.000000000000000000, 0.000000000000000000 ) ) ;
#5770 = DIRECTION ( 'NONE',  ( 0.000000000000000000, -1.000000000000000000, 0.000000000000000000 ) ) ;
#5771 = CARTESIAN_POINT ( 'NONE',  ( -29.37540678000427619, -6.000000000000000000, 7.200000000000000178 ) ) ;
#5772 = CARTESIAN_POINT ( 'NONE',  ( 31.50000000000002132, 71.00000000000001421, 3.200000000000000178 ) ) ;
#5773 = DIRECTION ( 'NONE',  ( 2.107255972849994642E-16, -0.000000000000000000, 1.000000000000000000 ) ) ;
#5774 = CARTESIAN_POINT ( 'NONE',  ( -25.37540678000427263, 69.04634676501045476, 3.500000000000000000 ) ) ;
#5775 = CARTESIAN_POINT ( 'NONE',  ( 28.57540678000427548, -6.776800961815481195, 13.50000000000000000 ) ) ;
#5776 = AXIS2_PLACEMENT_3D ( 'NONE', #14622, #16286, #21359 ) ;
#5777 = FACE_OUTER_BOUND ( 'NONE', #502, .T. ) ;
#5778 = DIRECTION ( 'NONE',  ( -1.000000000000000000, 0.000000000000000000, 0.000000000000000000 ) ) ;
#5779 = ADVANCED_FACE ( 'NONE', ( #11166 ), #9833, .T. ) ;
#5780 = ORIENTED_EDGE ( 'NONE', *, *, #14502, .F. ) ;
#5781 = ADVANCED_FACE ( 'NONE', ( #17989 ), #16190, .T. ) ;
#5782 = ORIENTED_EDGE ( 'NONE', *, *, #12390, .F. ) ;
#5783 = ORIENTED_EDGE ( 'NONE', *, *, #12126, .T. ) ;
#5784 = FACE_OUTER_BOUND ( 'NONE', #998, .T. ) ;
#5785 = DIRECTION ( 'NONE',  ( 0.000000000000000000, 0.000000000000000000, 1.000000000000000000 ) ) ;
#5786 = CARTESIAN_POINT ( 'NONE',  ( 30.67540678000428045, 0.000000000000000000, 3.799999999999999822 ) ) ;
#5787 = EDGE_CURVE ( 'NONE', #5534, #15636, #20577, .T. ) ;
#5788 = CIRCLE ( 'NONE', #14334, 3.200000000000001510 ) ;
#5789 = TOROIDAL_SURFACE ( 'NONE', #8984, 0.05000000000000000278, 0.05000000000000000278 ) ;
#5790 = ORIENTED_EDGE ( 'NONE', *, *, #2210, .F. ) ;
#5791 = CARTESIAN_POINT ( 'NONE',  ( -31.44597781366222122, 56.94165929845684815, 68.75000000000000000 ) ) ;
#5792 = DIRECTION ( 'NONE',  ( 0.000000000000000000, -0.000000000000000000, 1.000000000000000000 ) ) ;
#5793 = VERTEX_POINT ( 'NONE', #864 ) ;
#5794 = DIRECTION ( 'NONE',  ( 1.000000000000000000, 0.000000000000000000, -2.388292521039847891E-16 ) ) ;
#5795 = DIRECTION ( 'NONE',  ( 0.000000000000000000, -0.000000000000000000, 1.000000000000000000 ) ) ;
#5796 = DIRECTION ( 'NONE',  ( 0.000000000000000000, 0.000000000000000000, -1.000000000000000000 ) ) ;
#5797 = LINE ( 'NONE', #12248, #9497 ) ;
#5798 = ORIENTED_EDGE ( 'NONE', *, *, #4832, .F. ) ;
#5799 = CARTESIAN_POINT ( 'NONE',  ( 25.37540678000427263, 63.74634676501045050, 7.200000000000000178 ) ) ;
#5800 = CYLINDRICAL_SURFACE ( 'NONE', #11730, 0.2999999999999999334 ) ;
#5801 = DIRECTION ( 'NONE',  ( 0.000000000000000000, -0.000000000000000000, -1.000000000000000000 ) ) ;
#5802 = DIRECTION ( 'NONE',  ( -0.000000000000000000, 0.000000000000000000, 1.000000000000000000 ) ) ;
#5803 = ORIENTED_EDGE ( 'NONE', *, *, #18415, .T. ) ;
#5804 = AXIS2_PLACEMENT_3D ( 'NONE', #8709, #12038, #15504 ) ;
#5805 = ADVANCED_FACE ( 'NONE', ( #2904 ), #11505, .T. ) ;
#5806 = AXIS2_PLACEMENT_3D ( 'NONE', #13084, #20259, #1341 ) ;
#5807 = VERTEX_POINT ( 'NONE', #19796 ) ;
#5808 = AXIS2_PLACEMENT_3D ( 'NONE', #1211, #9634, #8061 ) ;
#5809 = CARTESIAN_POINT ( 'NONE',  ( 1.724728116533979616, 42.36054587065083155, 39.75876104995654003 ) ) ;
#5810 = AXIS2_PLACEMENT_3D ( 'NONE', #4750, #2848, #11550 ) ;
#5811 = DIRECTION ( 'NONE',  ( -0.000000000000000000, 0.000000000000000000, -1.000000000000000000 ) ) ;
#5812 = ORIENTED_EDGE ( 'NONE', *, *, #13810, .T. ) ;
#5813 = ORIENTED_EDGE ( 'NONE', *, *, #11151, .F. ) ;
#5814 = CYLINDRICAL_SURFACE ( 'NONE', #4231, 0.3000000000000003775 ) ;
#5815 = ORIENTED_EDGE ( 'NONE', *, *, #20966, .F. ) ;
#5816 = EDGE_CURVE ( 'NONE', #20280, #20277, #18099, .T. ) ;
#5817 = EDGE_CURVE ( 'NONE', #6556, #22161, #3407, .T. ) ;
#5818 = ORIENTED_EDGE ( 'NONE', *, *, #13992, .T. ) ;
#5819 = AXIS2_PLACEMENT_3D ( 'NONE', #12718, #17773, #9494 ) ;
#5820 = VERTEX_POINT ( 'NONE', #21600 ) ;
#5821 = CARTESIAN_POINT ( 'NONE',  ( -21.91689697940243775, 45.66657467514198743, 13.75000000000000000 ) ) ;
#5822 = AXIS2_PLACEMENT_3D ( 'NONE', #5018, #15612, #18888 ) ;
#5823 = CARTESIAN_POINT ( 'NONE',  ( -1.724728116533986721, 43.26054587065083012, 53.76679706732590347 ) ) ;
#5824 = DIRECTION ( 'NONE',  ( 0.000000000000000000, 0.000000000000000000, -1.000000000000000000 ) ) ;
#5825 = DIRECTION ( 'NONE',  ( 1.000000000000000000, 0.000000000000000000, -0.000000000000000000 ) ) ;
#5826 = DIRECTION ( 'NONE',  ( 1.000000000000000000, 0.000000000000000000, 0.000000000000000000 ) ) ;
#5827 = DIRECTION ( 'NONE',  ( 1.224646799147353207E-16, 0.000000000000000000, 1.000000000000000000 ) ) ;
#5828 = ORIENTED_EDGE ( 'NONE', *, *, #5765, .T. ) ;
#5829 = CARTESIAN_POINT ( 'NONE',  ( 15.05486995871383016, 52.39333383871512240, 13.50000000000000533 ) ) ;
#5830 = CIRCLE ( 'NONE', #801, 2.274596669241483848 ) ;
#5831 = EDGE_CURVE ( 'NONE', #4245, #21143, #18778, .T. ) ;
#5832 = CARTESIAN_POINT ( 'NONE',  ( -33.20000000000000284, 85.00000000000000000, 1.800000000000000266 ) ) ;
#5833 = FACE_OUTER_BOUND ( 'NONE', #17376, .T. ) ;
#5834 = ORIENTED_EDGE ( 'NONE', *, *, #2157, .F. ) ;
#5835 = CARTESIAN_POINT ( 'NONE',  ( 1.724728116533979838, 43.26054587065083012, 33.71679706732589921 ) ) ;
#5836 = ORIENTED_EDGE ( 'NONE', *, *, #18376, .T. ) ;
#5837 = ORIENTED_EDGE ( 'NONE', *, *, #11445, .F. ) ;
#5838 = ORIENTED_EDGE ( 'NONE', *, *, #1332, .T. ) ;
#5839 = CARTESIAN_POINT ( 'NONE',  ( -25.37540678000426908, 36.74634676501047181, 42.50000000000000000 ) ) ;
#5840 = ADVANCED_FACE ( 'NONE', ( #4909 ), #16618, .T. ) ;
#5841 = VERTEX_POINT ( 'NONE', #9948 ) ;
#5842 = EDGE_CURVE ( 'NONE', #16243, #12515, #1249, .T. ) ;
#5843 = ORIENTED_EDGE ( 'NONE', *, *, #5654, .F. ) ;
#5844 = EDGE_CURVE ( 'NONE', #8484, #11913, #3234, .T. ) ;
#5845 = DIRECTION ( 'NONE',  ( -0.000000000000000000, -0.000000000000000000, 1.000000000000000000 ) ) ;
#5846 = ORIENTED_EDGE ( 'NONE', *, *, #15150, .F. ) ;
#5847 = DIRECTION ( 'NONE',  ( -0.000000000000000000, 0.000000000000000000, 1.000000000000000000 ) ) ;
#5848 = ORIENTED_EDGE ( 'NONE', *, *, #3847, .F. ) ;
#5849 = CARTESIAN_POINT ( 'NONE',  ( -30.19999999999999574, 70.29999999999999716, 1.199999999999999512 ) ) ;
#5850 = CARTESIAN_POINT ( 'NONE',  ( -33.20000000000001705, 84.70000000000001705, 78.50000000000000000 ) ) ;
#5851 = DIRECTION ( 'NONE',  ( -1.000000000000000000, 0.000000000000000000, 0.000000000000000000 ) ) ;
#5852 = PLANE ( 'NONE',  #18961 ) ;
#5853 = ADVANCED_FACE ( 'NONE', ( #1312 ), #15083, .F. ) ;
#5854 = DIRECTION ( 'NONE',  ( 0.000000000000000000, -1.000000000000000000, 0.000000000000000000 ) ) ;
#5855 = CARTESIAN_POINT ( 'NONE',  ( -3.127054932750481964, -32.61873716947361856, 68.00000000000000000 ) ) ;
#5856 = FACE_OUTER_BOUND ( 'NONE', #7263, .T. ) ;
#5857 = DIRECTION ( 'NONE',  ( 0.000000000000000000, 1.000000000000000000, 0.000000000000000000 ) ) ;
#5858 = ORIENTED_EDGE ( 'NONE', *, *, #11046, .T. ) ;
#5859 = ORIENTED_EDGE ( 'NONE', *, *, #2148, .T. ) ;
#5860 = DIRECTION ( 'NONE',  ( 1.000000000000000000, 0.000000000000000000, 0.000000000000000000 ) ) ;
#5861 = EDGE_LOOP ( 'NONE', ( #8108, #6541, #4406, #9313 ) ) ;
#5862 = EDGE_CURVE ( 'NONE', #12755, #5867, #19851, .T. ) ;
#5863 = ORIENTED_EDGE ( 'NONE', *, *, #14540, .T. ) ;
#5864 = VERTEX_POINT ( 'NONE', #6497 ) ;
#5865 = ADVANCED_FACE ( 'NONE', ( #13292 ), #18552, .T. ) ;
#5866 = CARTESIAN_POINT ( 'NONE',  ( -1.824728116533986810, 42.36054587065083155, 41.66679706732590915 ) ) ;
#5867 = VERTEX_POINT ( 'NONE', #8088 ) ;
#5868 = LINE ( 'NONE', #3856, #5236 ) ;
#5869 = ORIENTED_EDGE ( 'NONE', *, *, #18806, .T. ) ;
#5870 = CARTESIAN_POINT ( 'NONE',  ( 15.95292532278785913, 50.11873716947361856, 109.6002446535588319 ) ) ;
#5871 = CARTESIAN_POINT ( 'NONE',  ( -1.774728116533986766, 43.31054587065082728, 29.66679706732590560 ) ) ;
#5872 = CARTESIAN_POINT ( 'NONE',  ( 15.07117748393522483, 52.06955913406978453, 13.87289863735440321 ) ) ;
#5873 = FACE_OUTER_BOUND ( 'NONE', #10495, .T. ) ;
#5874 = CARTESIAN_POINT ( 'NONE',  ( 1.724728116533979838, 43.26054587065083012, 53.66679706732590915 ) ) ;
#5875 = EDGE_CURVE ( 'NONE', #20894, #13259, #3767, .T. ) ;
#5876 = ORIENTED_EDGE ( 'NONE', *, *, #5067, .T. ) ;
#5877 = CARTESIAN_POINT ( 'NONE',  ( 28.79994065384636315, -6.566898051583388352, 13.40260211333369256 ) ) ;
#5878 = CARTESIAN_POINT ( 'NONE',  ( -9.178906393579158163, 42.46645089659918426, 70.38908280829822672 ) ) ;
#5879 = EDGE_CURVE ( 'NONE', #5378, #21318, #6941, .T. ) ;
#5880 = DIRECTION ( 'NONE',  ( 0.000000000000000000, 0.000000000000000000, 1.000000000000000000 ) ) ;
#5881 = ORIENTED_EDGE ( 'NONE', *, *, #19015, .T. ) ;
#5882 = ORIENTED_EDGE ( 'NONE', *, *, #466, .F. ) ;
#5883 = ORIENTED_EDGE ( 'NONE', *, *, #21949, .T. ) ;
#5884 = LINE ( 'NONE', #12565, #20285 ) ;
#5885 = DIRECTION ( 'NONE',  ( 0.4461977533474358326, 1.557891129246303114E-15, 0.8949343913984425525 ) ) ;
#5886 = ORIENTED_EDGE ( 'NONE', *, *, #12607, .T. ) ;
#5887 = CARTESIAN_POINT ( 'NONE',  ( 1.724728116533979838, 43.31054587065082728, 29.66679706732590560 ) ) ;
#5888 = CIRCLE ( 'NONE', #16935, 0.05000000000000143219 ) ;
#5889 = VERTEX_POINT ( 'NONE', #1773 ) ;
#5890 = PLANE ( 'NONE',  #13968 ) ;
#5891 = DIRECTION ( 'NONE',  ( 0.000000000000000000, -0.000000000000000000, 1.000000000000000000 ) ) ;
#5892 = DIRECTION ( 'NONE',  ( 6.123233995736764803E-17, -0.000000000000000000, -1.000000000000000000 ) ) ;
#5893 = DIRECTION ( 'NONE',  ( -1.327594496921025717E-16, -1.000000000000000000, 1.625834351219974904E-32 ) ) ;
#5894 = CARTESIAN_POINT ( 'NONE',  ( -27.67540678000426269, 36.74634676501047181, 13.79999999999999893 ) ) ;
#5895 = CARTESIAN_POINT ( 'NONE',  ( 14.96174975910707161, -41.81054587065082728, 68.25000000000000000 ) ) ;
#5896 = EDGE_LOOP ( 'NONE', ( #12901, #21566, #15795, #11204 ) ) ;
#5897 = CARTESIAN_POINT ( 'NONE',  ( -9.178906393579158163, 42.46645089659918426, 70.88527860057354246 ) ) ;
#5898 = DIRECTION ( 'NONE',  ( -1.734723475976806848E-16, 0.000000000000000000, 1.000000000000000000 ) ) ;
#5899 = DIRECTION ( 'NONE',  ( 1.000000000000000000, 0.000000000000000000, 0.000000000000000000 ) ) ;
#5900 = CYLINDRICAL_SURFACE ( 'NONE', #17120, 0.2500000000000002220 ) ;
#5901 = VERTEX_POINT ( 'NONE', #11721 ) ;
#5902 = DIRECTION ( 'NONE',  ( -0.000000000000000000, -1.000000000000000000, 0.000000000000000000 ) ) ;
#5903 = ORIENTED_EDGE ( 'NONE', *, *, #8733, .F. ) ;
#5904 = CARTESIAN_POINT ( 'NONE',  ( -9.178906393579158163, 42.46645089659918426, 68.75385983073485363 ) ) ;
#5905 = DIRECTION ( 'NONE',  ( 0.000000000000000000, 0.000000000000000000, 1.000000000000000000 ) ) ;
#5906 = EDGE_CURVE ( 'NONE', #22033, #19724, #11600, .T. ) ;
#5907 = ORIENTED_EDGE ( 'NONE', *, *, #7981, .F. ) ;
#5908 = VERTEX_POINT ( 'NONE', #18898 ) ;
#5909 = DIRECTION ( 'NONE',  ( 0.000000000000000000, -1.000000000000000000, 0.000000000000000000 ) ) ;
#5910 = CARTESIAN_POINT ( 'NONE',  ( -1.724728116533986721, 43.26054587065083012, 37.66679706732590915 ) ) ;
#5911 = CARTESIAN_POINT ( 'NONE',  ( 0.000000000000000000, -39.04634676501046187, 13.50000000000000000 ) ) ;
#5912 = ORIENTED_EDGE ( 'NONE', *, *, #9196, .T. ) ;
#5913 = ORIENTED_EDGE ( 'NONE', *, *, #19560, .T. ) ;
#5914 = CIRCLE ( 'NONE', #1946, 0.4999999999999995559 ) ;
#5915 = AXIS2_PLACEMENT_3D ( 'NONE', #8717, #7482, #14280 ) ;
#5916 = VERTEX_POINT ( 'NONE', #16977 ) ;
#5917 = CARTESIAN_POINT ( 'NONE',  ( -26.56227312273159313, -9.958410664601842655, 13.79999999999999893 ) ) ;
#5918 = ADVANCED_FACE ( 'NONE', ( #8612 ), #10190, .F. ) ;
#5919 = B_SPLINE_CURVE_WITH_KNOTS ( 'NONE', 3,
 ( #12556, #7226, #19401, #9007, #15908, #17608, #16134, #2053 ),
 .UNSPECIFIED., .F., .F.,
 ( 4, 2, 2, 4 ),
 ( 0.000000000000000000, 0.0004685292328704453928, 0.0007027938493056759767, 0.0009370584657409066149 ),
 .UNSPECIFIED. ) ;
#5920 = FACE_OUTER_BOUND ( 'NONE', #18029, .T. ) ;
#5921 = DIRECTION ( 'NONE',  ( 0.000000000000000000, 0.000000000000000000, 1.000000000000000000 ) ) ;
#5922 = CARTESIAN_POINT ( 'NONE',  ( -9.978973617317260292, 41.92645089659918511, 68.06527860057354928 ) ) ;
#5923 = CARTESIAN_POINT ( 'NONE',  ( 0.000000000000000000, 42.31054587065082728, 31.75876104995653648 ) ) ;
#5924 = CARTESIAN_POINT ( 'NONE',  ( -9.178906393579158163, 42.46645089659918426, 68.06527860057354928 ) ) ;
#5925 = ORIENTED_EDGE ( 'NONE', *, *, #20739, .T. ) ;
#5926 = CARTESIAN_POINT ( 'NONE',  ( -1.724728116533986721, 42.36054587065083155, 53.66679706732590915 ) ) ;
#5927 = AXIS2_PLACEMENT_3D ( 'NONE', #9733, #7950, #12715 ) ;
#5928 = EDGE_CURVE ( 'NONE', #3824, #19461, #22036, .T. ) ;
#5929 = DIRECTION ( 'NONE',  ( -0.000000000000000000, -0.000000000000000000, -1.000000000000000000 ) ) ;
#5930 = FACE_OUTER_BOUND ( 'NONE', #17305, .T. ) ;
#5931 = TOROIDAL_SURFACE ( 'NONE', #7699, 0.7000000000000000666, 0.2999999999999999889 ) ;
#5932 = CIRCLE ( 'NONE', #1632, 0.5000000000000004441 ) ;
#5933 = AXIS2_PLACEMENT_3D ( 'NONE', #1064, #1270, #6229 ) ;
#5934 = CARTESIAN_POINT ( 'NONE',  ( -23.61959064016851073, 45.26242829375641463, 68.50000000000000000 ) ) ;
#5935 = DIRECTION ( 'NONE',  ( 2.107255972849994642E-16, -0.000000000000000000, 1.000000000000000000 ) ) ;
#5936 = ORIENTED_EDGE ( 'NONE', *, *, #11341, .F. ) ;
#5937 = ORIENTED_EDGE ( 'NONE', *, *, #17035, .F. ) ;
#5938 = ORIENTED_EDGE ( 'NONE', *, *, #13781, .T. ) ;
#5939 = CARTESIAN_POINT ( 'NONE',  ( 15.95292532278785913, -50.11873716947361856, 109.6002446535588319 ) ) ;
#5940 = CONTEXT_DEPENDENT_SHAPE_REPRESENTATION ( #8871, #13747 ) ;
#5941 = ORIENTED_EDGE ( 'NONE', *, *, #21708, .T. ) ;
#5942 = ORIENTED_EDGE ( 'NONE', *, *, #9569, .T. ) ;
#5943 = AXIS2_PLACEMENT_3D ( 'NONE', #2086, #21008, #10918 ) ;
#5944 = AXIS2_PLACEMENT_3D ( 'NONE', #13682, #20186, #14920 ) ;
#5945 = AXIS2_PLACEMENT_3D ( 'NONE', #3712, #19048, #21070 ) ;
#5946 = EDGE_CURVE ( 'NONE', #1910, #7925, #8374, .T. ) ;
#5947 = ORIENTED_EDGE ( 'NONE', *, *, #13979, .F. ) ;
#5948 = DIRECTION ( 'NONE',  ( -0.000000000000000000, 1.000000000000000000, -0.000000000000000000 ) ) ;
#5949 = CIRCLE ( 'NONE', #17708, 0.5000000000000004441 ) ;
#5950 = VECTOR ( 'NONE', #19174, 1000.000000000000000 ) ;
#5951 = FACE_OUTER_BOUND ( 'NONE', #763, .T. ) ;
#5952 = DIRECTION ( 'NONE',  ( -1.000000000000000000, 0.000000000000000000, 0.000000000000000000 ) ) ;
#5953 = DIRECTION ( 'NONE',  ( -0.000000000000000000, 1.000000000000000000, -0.000000000000000000 ) ) ;
#5954 = DIRECTION ( 'NONE',  ( -0.000000000000000000, -0.000000000000000000, -1.000000000000000000 ) ) ;
#5955 = EDGE_CURVE ( 'NONE', #16035, #18107, #11962, .T. ) ;
#5956 = DIRECTION ( 'NONE',  ( 1.000000000000000000, -1.094601647044990554E-16, 0.000000000000000000 ) ) ;
#5957 = EDGE_CURVE ( 'NONE', #21291, #1963, #18665, .T. ) ;
#5958 = LINE ( 'NONE', #12747, #13996 ) ;
#5959 = DIRECTION ( 'NONE',  ( 0.000000000000000000, 0.000000000000000000, 1.000000000000000000 ) ) ;
#5960 = CIRCLE ( 'NONE', #14139, 0.2500000000000004996 ) ;
#5961 = VECTOR ( 'NONE', #632, 1000.000000000000000 ) ;
#5962 = TOROIDAL_SURFACE ( 'NONE', #9882, 1.750000000000000000, 0.2500000000000000000 ) ;
#5963 = EDGE_CURVE ( 'NONE', #1986, #1398, #22159, .T. ) ;
#5964 = CARTESIAN_POINT ( 'NONE',  ( 9.641460742840918030, 32.11873716947361856, 42.50000000000000711 ) ) ;
#5965 = FACE_OUTER_BOUND ( 'NONE', #1381, .T. ) ;
#5966 = ORIENTED_EDGE ( 'NONE', *, *, #1669, .T. ) ;
#5967 = VECTOR ( 'NONE', #1227, 1000.000000000000000 ) ;
#5968 = EDGE_LOOP ( 'NONE', ( #12050, #21790, #18403, #9875 ) ) ;
#5969 = CARTESIAN_POINT ( 'NONE',  ( 30.49999999999999645, 70.29999999999999716, 1.200000000000003064 ) ) ;
#5970 = DIRECTION ( 'NONE',  ( 0.000000000000000000, 0.000000000000000000, 1.000000000000000000 ) ) ;
#5971 = ORIENTED_EDGE ( 'NONE', *, *, #17818, .F. ) ;
#5972 = ORIENTED_EDGE ( 'NONE', *, *, #19934, .T. ) ;
#5973 = EDGE_CURVE ( 'NONE', #16645, #16312, #13626, .T. ) ;
#5974 = AXIS2_PLACEMENT_3D ( 'NONE', #7791, #1836, #1500 ) ;
#5975 = VECTOR ( 'NONE', #20895, 1000.000000000000000 ) ;
#5976 = VECTOR ( 'NONE', #21849, 1000.000000000000000 ) ;
#5977 = VECTOR ( 'NONE', #12945, 1000.000000000000000 ) ;
#5978 = CARTESIAN_POINT ( 'NONE',  ( -23.36959064016851073, 45.26242829375641463, 68.25000000000000000 ) ) ;
#5979 = AXIS2_PLACEMENT_3D ( 'NONE', #17457, #743, #8741 ) ;
#5980 = ORIENTED_EDGE ( 'NONE', *, *, #14451, .F. ) ;
#5981 = SURFACE_SIDE_STYLE ('',( #12991 ) ) ;
#5982 = DIRECTION ( 'NONE',  ( 1.000000000000000000, 0.000000000000000000, 0.000000000000000000 ) ) ;
#5983 = ADVANCED_FACE ( 'NONE', ( #13722 ), #8165, .F. ) ;
#5984 = DIRECTION ( 'NONE',  ( 0.000000000000000000, 1.000000000000000000, 0.000000000000000000 ) ) ;
#5985 = CARTESIAN_POINT ( 'NONE',  ( -29.37540678000427619, -5.000000000000000000, 3.799999999999999822 ) ) ;
#5986 = CARTESIAN_POINT ( 'NONE',  ( -1.824728116533986810, 42.36054587065083155, 47.80876104995653719 ) ) ;
#5987 = MANIFOLD_SOLID_BREP ( 'Stock-MAS-696-1', #10645 ) ;
#5988 = EDGE_CURVE ( 'NONE', #11011, #4007, #13742, .T. ) ;
#5989 = VERTEX_POINT ( 'NONE', #21014 ) ;
#5990 = LINE ( 'NONE', #10796, #18272 ) ;
#5991 = FACE_OUTER_BOUND ( 'NONE', #21218, .T. ) ;
#5992 = AXIS2_PLACEMENT_3D ( 'NONE', #17348, #20731, #13991 ) ;
#5993 = DIRECTION ( 'NONE',  ( -0.000000000000000000, 0.000000000000000000, 1.000000000000000000 ) ) ;
#5994 = ORIENTED_EDGE ( 'NONE', *, *, #17066, .F. ) ;
#5995 = AXIS2_PLACEMENT_3D ( 'NONE', #1439, #8280, #11837 ) ;
#5996 = AXIS2_PLACEMENT_3D ( 'NONE', #14517, #12720, #4583 ) ;
#5997 = VERTEX_POINT ( 'NONE', #17537 ) ;
#5998 = CARTESIAN_POINT ( 'NONE',  ( -1.824728116533986810, 43.31054587065082728, 31.70876104995653932 ) ) ;
#5999 = LINE ( 'NONE', #10900, #11322 ) ;
#6000 = VERTEX_POINT ( 'NONE', #2092 ) ;
#6001 = AXIS2_PLACEMENT_3D ( 'NONE', #20524, #13900, #10778 ) ;
#6002 = LINE ( 'NONE', #6220, #2709 ) ;
#6003 = AXIS2_PLACEMENT_3D ( 'NONE', #11452, #19634, #18381 ) ;
#6004 = VECTOR ( 'NONE', #14778, 1000.000000000000000 ) ;
#6005 = ORIENTED_EDGE ( 'NONE', *, *, #15555, .T. ) ;
#6006 = CARTESIAN_POINT ( 'NONE',  ( -9.641460742840918030, -32.61873716947361856, 68.50000000000000000 ) ) ;
#6007 = CARTESIAN_POINT ( 'NONE',  ( -30.19999999999999574, 70.29999999999999716, 0.3000000000000002665 ) ) ;
#6008 = ADVANCED_FACE ( 'NONE', ( #2203 ), #19107, .T. ) ;
#6009 = LINE ( 'NONE', #941, #14575 ) ;
#6010 = CARTESIAN_POINT ( 'NONE',  ( -1.774728116533986766, 43.26054587065083012, 0.000000000000000000 ) ) ;
#6011 = CIRCLE ( 'NONE', #9203, 0.2999999999999999334 ) ;
#6012 = AXIS2_PLACEMENT_3D ( 'NONE', #15086, #20137, #5141 ) ;
#6013 = DIRECTION ( 'NONE',  ( -2.388292521039847891E-16, 0.000000000000000000, -1.000000000000000000 ) ) ;
#6014 = LINE ( 'NONE', #9796, #19490 ) ;
#6015 = EDGE_LOOP ( 'NONE', ( #13329, #11202, #1240, #12083 ) ) ;
#6016 = CARTESIAN_POINT ( 'NONE',  ( -35.00000000000001421, -84.70000000000001705, 78.50000000000000000 ) ) ;
#6017 = DIRECTION ( 'NONE',  ( 0.000000000000000000, 0.000000000000000000, -1.000000000000000000 ) ) ;
#6018 = AXIS2_PLACEMENT_3D ( 'NONE', #3691, #17653, #19241 ) ;
#6019 = CARTESIAN_POINT ( 'NONE',  ( -14.98825539710680310, 51.95771298364782353, 13.85621828746129403 ) ) ;
#6020 = DIRECTION ( 'NONE',  ( 1.000000000000000000, 0.000000000000000000, 0.000000000000000000 ) ) ;
#6021 = ORIENTED_EDGE ( 'NONE', *, *, #15249, .T. ) ;
#6022 = FACE_OUTER_BOUND ( 'NONE', #14642, .T. ) ;
#6023 = VECTOR ( 'NONE', #19828, 1000.000000000000000 ) ;
#6024 = DIRECTION ( 'NONE',  ( 1.000000000000000000, -0.000000000000000000, -0.000000000000000000 ) ) ;
#6025 = AXIS2_PLACEMENT_3D ( 'NONE', #1569, #5058, #21957 ) ;
#6026 = ADVANCED_FACE ( 'NONE', ( #14162 ), #10602, .F. ) ;
#6027 = EDGE_LOOP ( 'NONE', ( #3734, #7372, #10117, #11650 ) ) ;
#6028 = CARTESIAN_POINT ( 'NONE',  ( -17.92752199202934094, 50.11873716947361856, 13.79999999999999893 ) ) ;
#6029 = DIRECTION ( 'NONE',  ( 0.000000000000000000, -1.000000000000000000, 0.000000000000000000 ) ) ;
#6030 = VERTEX_POINT ( 'NONE', #9139 ) ;
#6031 = EDGE_LOOP ( 'NONE', ( #3241, #13865, #16098, #18745 ) ) ;
#6032 = CARTESIAN_POINT ( 'NONE',  ( -1.724728116533986721, 42.31054587065082728, 47.75876104995653293 ) ) ;
#6033 = CARTESIAN_POINT ( 'NONE',  ( -33.20000000000001705, -85.00000000000000000, 78.20000000000000284 ) ) ;
#6034 = AXIS2_PLACEMENT_3D ( 'NONE', #233, #762, #21155 ) ;
#6035 = EDGE_LOOP ( 'NONE', ( #18388, #9068, #10324, #9547 ) ) ;
#6036 = AXIS2_PLACEMENT_3D ( 'NONE', #9458, #14274, #17850 ) ;
#6037 = VERTEX_POINT ( 'NONE', #8928 ) ;
#6038 = LINE ( 'NONE', #4445, #4325 ) ;
#6039 = CIRCLE ( 'NONE', #2083, 0.2999999999999999334 ) ;
#6040 = AXIS2_PLACEMENT_3D ( 'NONE', #11927, #22150, #20459 ) ;
#6041 = EDGE_CURVE ( 'NONE', #5534, #513, #1971, .T. ) ;
#6042 = LINE ( 'NONE', #19676, #14191 ) ;
#6043 = CARTESIAN_POINT ( 'NONE',  ( 1.724728116533979616, 42.31054587065082728, 29.71679706732590631 ) ) ;
#6044 = EDGE_CURVE ( 'NONE', #10547, #2324, #22002, .T. ) ;
#6045 = DIRECTION ( 'NONE',  ( -0.000000000000000000, -1.000000000000000000, -0.000000000000000000 ) ) ;
#6046 = CARTESIAN_POINT ( 'NONE',  ( -34.70000000000001705, -84.70000000000001705, 79.39999999999999147 ) ) ;
#6047 = CARTESIAN_POINT ( 'NONE',  ( 1.724728116533979616, 42.36054587065083155, 43.80876104995653719 ) ) ;
#6048 = CARTESIAN_POINT ( 'NONE',  ( -17.93704824106378837, 0.000000000000000000, 13.87500000000000000 ) ) ;
#6049 = DIRECTION ( 'NONE',  ( 0.000000000000000000, 1.000000000000000000, 0.000000000000000000 ) ) ;
#6050 = ORIENTED_EDGE ( 'NONE', *, *, #16425, .T. ) ;
#6051 = CIRCLE ( 'NONE', #16018, 0.04999999999999991257 ) ;
#6052 = LINE ( 'NONE', #21706, #8063 ) ;
#6053 = DIRECTION ( 'NONE',  ( -0.000000000000000000, 0.000000000000000000, 1.000000000000000000 ) ) ;
#6054 = AXIS2_PLACEMENT_3D ( 'NONE', #9354, #21126, #21338 ) ;
#6055 = CARTESIAN_POINT ( 'NONE',  ( -8.641460742840918030, 32.93424481021354921, 68.00000000000000000 ) ) ;
#6056 = AXIS2_PLACEMENT_3D ( 'NONE', #17209, #3784, #9046 ) ;
#6057 = FACE_OUTER_BOUND ( 'NONE', #21636, .T. ) ;
#6058 = VERTEX_POINT ( 'NONE', #9039 ) ;
#6059 = ADVANCED_FACE ( 'NONE', ( #407 ), #9112, .T. ) ;
#6060 = ORIENTED_EDGE ( 'NONE', *, *, #654, .T. ) ;
#6061 = DIRECTION ( 'NONE',  ( 1.000000000000000000, -0.000000000000000000, -0.000000000000000000 ) ) ;
#6062 = SHAPE_DEFINITION_REPRESENTATION ( #21629, #6277 ) ;
#6063 = ORIENTED_EDGE ( 'NONE', *, *, #14513, .F. ) ;
#6064 = ORIENTED_EDGE ( 'NONE', *, *, #9266, .F. ) ;
#6065 = EDGE_CURVE ( 'NONE', #3680, #538, #9482, .T. ) ;
#6066 = CARTESIAN_POINT ( 'NONE',  ( -25.37540678000427263, -67.24634676501045760, 13.19999999999999929 ) ) ;
#6067 = ORIENTED_EDGE ( 'NONE', *, *, #20063, .T. ) ;
#6068 = DIRECTION ( 'NONE',  ( 1.000000000000000000, 0.000000000000000000, 0.000000000000000000 ) ) ;
#6069 = AXIS2_PLACEMENT_3D ( 'NONE', #3805, #1520, #5004 ) ;
#6070 = AXIS2_PLACEMENT_3D ( 'NONE', #6268, #11396, #13057 ) ;
#6071 = DIRECTION ( 'NONE',  ( -0.000000000000000000, 1.000000000000000000, -0.000000000000000000 ) ) ;
#6072 = DIRECTION ( 'NONE',  ( 1.000000000000000000, 0.000000000000000000, 0.000000000000000000 ) ) ;
#6073 = CARTESIAN_POINT ( 'NONE',  ( -29.13662752439705272, 5.299999999999999822, 7.500000000000000000 ) ) ;
#6074 = LINE ( 'NONE', #2478, #4310 ) ;
#6075 = CYLINDRICAL_SURFACE ( 'NONE', #15804, 0.05000000000000143219 ) ;
#6076 = LINE ( 'NONE', #12863, #19729 ) ;
#6077 = CYLINDRICAL_SURFACE ( 'NONE', #3753, 0.05000000000000143219 ) ;
#6078 = CARTESIAN_POINT ( 'NONE',  ( 0.000000000000000000, -5.000000000000000000, 7.200000000000000178 ) ) ;
#6079 = AXIS2_PLACEMENT_3D ( 'NONE', #18858, #3642, #5209 ) ;
#6080 = ADVANCED_FACE ( 'NONE', ( #13834 ), #20691, .T. ) ;
#6081 = VERTEX_POINT ( 'NONE', #7151 ) ;
#6082 = DIRECTION ( 'NONE',  ( -1.000000000000000000, -3.543406725251269872E-15, 1.224646799147353207E-16 ) ) ;
#6083 = CIRCLE ( 'NONE', #8137, 0.04999999999999991257 ) ;
#6084 = DIRECTION ( 'NONE',  ( -2.107255972849994642E-16, 0.000000000000000000, -1.000000000000000000 ) ) ;
#6085 = ORIENTED_EDGE ( 'NONE', *, *, #5403, .T. ) ;
#6086 = ORIENTED_EDGE ( 'NONE', *, *, #4967, .F. ) ;
#6087 = CARTESIAN_POINT ( 'NONE',  ( 15.21174975910707161, -51.61873716947361856, 68.00000000000000000 ) ) ;
#6088 = ORIENTED_EDGE ( 'NONE', *, *, #10656, .T. ) ;
#6089 = DIRECTION ( 'NONE',  ( 0.000000000000000000, -1.000000000000000000, 0.000000000000000000 ) ) ;
#6090 = EDGE_LOOP ( 'NONE', ( #15849, #6067, #15969, #13031 ) ) ;
#6091 = ADVANCED_FACE ( 'NONE', ( #7258 ), #20797, .T. ) ;
#6092 = EDGE_CURVE ( 'NONE', #675, #17770, #2322, .T. ) ;
#6093 = ADVANCED_FACE ( 'NONE', ( #17855 ), #11607, .T. ) ;
#6094 = FACE_OUTER_BOUND ( 'NONE', #18726, .T. ) ;
#6095 = COLOUR_RGB ( '', 0.72549020, 0.75294118, 0.79215686) ;
#6096 = DIRECTION ( 'NONE',  ( -1.000000000000000000, 0.000000000000000000, 0.000000000000000000 ) ) ;
#6097 = ORIENTED_EDGE ( 'NONE', *, *, #4358, .F. ) ;
#6098 = CYLINDRICAL_SURFACE ( 'NONE', #13974, 1.000000000000000888 ) ;
#6099 = CARTESIAN_POINT ( 'NONE',  ( 15.05577974591271051, 52.39333374568191459, 13.50000000000000000 ) ) ;
#6100 = DIRECTION ( 'NONE',  ( 0.000000000000000000, 1.000000000000000000, 0.000000000000000000 ) ) ;
#6101 = DIRECTION ( 'NONE',  ( -0.000000000000000000, -0.000000000000000000, -1.000000000000000000 ) ) ;
#6102 = EDGE_CURVE ( 'NONE', #8942, #6383, #954, .T. ) ;
#6103 = ORIENTED_EDGE ( 'NONE', *, *, #3040, .T. ) ;
#6104 = DIRECTION ( 'NONE',  ( 0.000000000000000000, -0.000000000000000000, 1.000000000000000000 ) ) ;
#6105 = DIRECTION ( 'NONE',  ( -1.000000000000000000, 0.000000000000000000, 0.000000000000000000 ) ) ;
#6106 = ORIENTED_EDGE ( 'NONE', *, *, #10518, .T. ) ;
#6107 = ORIENTED_EDGE ( 'NONE', *, *, #3251, .F. ) ;
#6108 = EDGE_LOOP ( 'NONE', ( #18295, #11813, #7511, #10817 ) ) ;
#6109 = DIRECTION ( 'NONE',  ( 0.000000000000000000, 0.000000000000000000, -1.000000000000000000 ) ) ;
#6110 = VECTOR ( 'NONE', #5948, 1000.000000000000000 ) ;
#6111 = CARTESIAN_POINT ( 'NONE',  ( 3.627054932750481964, 32.61873716947361856, 68.00000000000000000 ) ) ;
#6112 = ORIENTED_EDGE ( 'NONE', *, *, #15959, .F. ) ;
#6113 = CIRCLE ( 'NONE', #10034, 1.974596669241483804 ) ;
#6114 = DIRECTION ( 'NONE',  ( -1.224646799147353207E-16, -1.000000000000000000, 0.000000000000000000 ) ) ;
#6115 = ADVANCED_FACE ( 'NONE', ( #7919 ), #2876, .F. ) ;
#6116 = EDGE_CURVE ( 'NONE', #803, #8243, #17328, .T. ) ;
#6117 = ORIENTED_EDGE ( 'NONE', *, *, #18421, .F. ) ;
#6118 = CARTESIAN_POINT ( 'NONE',  ( 14.96174975910705918, -41.81054587065082728, 13.80000000000001315 ) ) ;
#6119 = B_SPLINE_CURVE_WITH_KNOTS ( 'NONE', 3,
 ( #6785, #11670, #16930, #1598, #18729, #8435, #6662, #22106 ),
 .UNSPECIFIED., .F., .F.,
 ( 4, 2, 2, 4 ),
 ( 0.000000000000000000, 0.0001199231866840693908, 0.0002398463733681387817, 0.0004796927467362803281 ),
 .UNSPECIFIED. ) ;
#6120 = CYLINDRICAL_SURFACE ( 'NONE', #13085, 0.05000000000000143219 ) ;
#6121 = EDGE_CURVE ( 'NONE', #18072, #1412, #12687, .T. ) ;
#6122 = LINE ( 'NONE', #16255, #11353 ) ;
#6123 = DIRECTION ( 'NONE',  ( -4.336808689941893885E-15, 0.000000000000000000, 1.000000000000000000 ) ) ;
#6124 = CYLINDRICAL_SURFACE ( 'NONE', #753, 0.5000000000000000000 ) ;
#6125 = CARTESIAN_POINT ( 'NONE',  ( 30.49999999999999645, 70.00000000000000000, 0.3000000000000033751 ) ) ;
#6126 = EDGE_LOOP ( 'NONE', ( #6169, #7014, #13291, #14291 ) ) ;
#6127 = DIRECTION ( 'NONE',  ( 1.000000000000000000, 0.000000000000000000, -2.388292521039847891E-16 ) ) ;
#6128 = CIRCLE ( 'NONE', #16106, 6.500000000000002665 ) ;
#6129 = CARTESIAN_POINT ( 'NONE',  ( -15.13056916446892153, 52.10286008774956201, 13.87500000000000000 ) ) ;
#6130 = CARTESIAN_POINT ( 'NONE',  ( -8.213656393579155335, 42.46645089659918426, 68.06527860057354928 ) ) ;
#6131 = ORIENTED_EDGE ( 'NONE', *, *, #21899, .T. ) ;
#6132 = FILL_AREA_STYLE ('',( #737 ) ) ;
#6133 = DIRECTION ( 'NONE',  ( 0.000000000000000000, 0.000000000000000000, 1.000000000000000000 ) ) ;
#6134 = EDGE_CURVE ( 'NONE', #21768, #17693, #2533, .T. ) ;
#6135 = ORIENTED_EDGE ( 'NONE', *, *, #1642, .T. ) ;
#6136 = DIRECTION ( 'NONE',  ( 0.000000000000000000, 1.000000000000000000, 0.000000000000000000 ) ) ;
#6137 = CARTESIAN_POINT ( 'NONE',  ( 0.000000000000000000, 43.26054587065083012, 41.71679706732590631 ) ) ;
#6138 = ORIENTED_EDGE ( 'NONE', *, *, #9768, .F. ) ;
#6139 = ORIENTED_EDGE ( 'NONE', *, *, #8396, .T. ) ;
#6140 = CARTESIAN_POINT ( 'NONE',  ( -15.13992500838820909, 52.10286008548567338, 13.87499999123205363 ) ) ;
#6141 = DIRECTION ( 'NONE',  ( 0.000000000000000000, 1.000000000000000000, 0.000000000000000000 ) ) ;
#6142 = EDGE_CURVE ( 'NONE', #2469, #9565, #12313, .T. ) ;
#6143 = CARTESIAN_POINT ( 'NONE',  ( 1.824728116533979261, 42.36054587065083155, 35.70876104995653577 ) ) ;
#6144 = CIRCLE ( 'NONE', #3992, 0.04999999999999991257 ) ;
#6145 = ORIENTED_EDGE ( 'NONE', *, *, #5423, .F. ) ;
#6146 = CIRCLE ( 'NONE', #8993, 0.2999999999999999334 ) ;
#6147 = ORIENTED_EDGE ( 'NONE', *, *, #22026, .F. ) ;
#6148 = CARTESIAN_POINT ( 'NONE',  ( 1.724728116533979838, 42.36054587065083155, 53.66679706732590915 ) ) ;
#6149 = EDGE_CURVE ( 'NONE', #17036, #9183, #21677, .T. ) ;
#6150 = DIRECTION ( 'NONE',  ( 0.000000000000000000, 0.000000000000000000, -1.000000000000000000 ) ) ;
#6151 = DIRECTION ( 'NONE',  ( 0.000000000000000000, 0.000000000000000000, -1.000000000000000000 ) ) ;
#6152 = AXIS2_PLACEMENT_3D ( 'NONE', #15699, #5663, #372 ) ;
#6153 = CARTESIAN_POINT ( 'NONE',  ( 29.69597781366221767, 27.99124249474150972, 68.75000000000000000 ) ) ;
#6154 = CARTESIAN_POINT ( 'NONE',  ( 1.774728116533979438, 43.31054587065082728, 39.80876104995653719 ) ) ;
#6155 = DIRECTION ( 'NONE',  ( 1.000000000000000000, 0.000000000000000000, 0.000000000000000000 ) ) ;
#6156 = DIRECTION ( 'NONE',  ( -1.000000000000000000, 0.000000000000000000, 0.000000000000000000 ) ) ;
#6157 = AXIS2_PLACEMENT_3D ( 'NONE', #9437, #16236, #2845 ) ;
#6158 = TOROIDAL_SURFACE ( 'NONE', #5076, 0.2999999999999999889, 0.2999999999999999889 ) ;
#6159 = LINE ( 'NONE', #16187, #4905 ) ;
#6160 = CARTESIAN_POINT ( 'NONE',  ( 30.79999999999999716, 69.70000000000000284, 1.500000000000004219 ) ) ;
#6161 = ORIENTED_EDGE ( 'NONE', *, *, #9644, .F. ) ;
#6162 =( BOUNDED_SURFACE ( )  B_SPLINE_SURFACE ( 3, 2, ( 
 ( #3700, #10524, #17332 ),
 ( #13973, #12695, #2004 ),
 ( #19548, #15657, #330 ),
 ( #5504, #18204, #2762 ),
 ( #16515, #13375, #21908 ),
 ( #21580, #1180, #16613 ),
 ( #6140, #21473, #21687 ),
 ( #2647, #3091, #11250 ) ),
 .UNSPECIFIED., .F., .F., .T. ) 
 B_SPLINE_SURFACE_WITH_KNOTS ( ( 4, 2, 2, 4 ),
 ( 3, 3 ),
 ( -1.016439536705160407E-20, 0.0002312589012449743479, 0.0004625178024899486958, 0.0009250356049798973915 ),
 ( 0.000000000000000000, 1.000000000000000000 ),
 .UNSPECIFIED. ) 
 GEOMETRIC_REPRESENTATION_ITEM ( )  RATIONAL_B_SPLINE_SURFACE ( (
 ( 1.000000000000000000, 0.7071067811865475727, 1.000000000000000000),
 ( 1.000000000000000000, 0.6819975405126383894, 1.000000000000000000),
 ( 1.000000000000000000, 0.6638073299468163491, 1.000000000000000000),
 ( 1.000000000000000000, 0.6387680821201728865, 1.000000000000000000),
 ( 1.000000000000000000, 0.6313903660824350395, 1.000000000000000000),
 ( 1.000000000000000000, 0.6152524581541630733, 1.000000000000000000),
 ( 1.000000000000000000, 0.6128152994388438302, 1.000000000000000000),
 ( 1.000000000000000000, 0.6123724356957929160, 1.000000000000000000) ) ) 
 REPRESENTATION_ITEM ( '' )  SURFACE ( )  );
#6163 = DIRECTION ( 'NONE',  ( 1.000000000000000000, 0.000000000000000000, 0.000000000000000000 ) ) ;
#6164 = FACE_OUTER_BOUND ( 'NONE', #8469, .T. ) ;
#6165 = CARTESIAN_POINT ( 'NONE',  ( 15.21174975910707161, 42.31054587065082728, 68.50000000000000000 ) ) ;
#6166 = ORIENTED_EDGE ( 'NONE', *, *, #8127, .F. ) ;
#6167 = EDGE_CURVE ( 'NONE', #19133, #6030, #7354, .T. ) ;
#6168 = LINE ( 'NONE', #17884, #10631 ) ;
#6169 = ORIENTED_EDGE ( 'NONE', *, *, #3779, .T. ) ;
#6170 = ADVANCED_FACE ( 'NONE', ( #10923 ), #1071, .T. ) ;
#6171 = ADVANCED_FACE ( 'NONE', ( #6022 ), #840, .F. ) ;
#6172 = VERTEX_POINT ( 'NONE', #19539 ) ;
#6173 = DIRECTION ( 'NONE',  ( -0.000000000000000000, 0.000000000000000000, 1.000000000000000000 ) ) ;
#6174 = AXIS2_PLACEMENT_3D ( 'NONE', #7636, #794, #1220 ) ;
#6175 = VERTEX_POINT ( 'NONE', #9588 ) ;
#6176 = AXIS2_PLACEMENT_3D ( 'NONE', #12829, #12388, #7501 ) ;
#6177 = DIRECTION ( 'NONE',  ( 0.000000000000000000, 0.000000000000000000, -1.000000000000000000 ) ) ;
#6178 = CARTESIAN_POINT ( 'NONE',  ( -9.978973617317267397, 43.00645089659918341, 68.06527860057354928 ) ) ;
#6179 = MANIFOLD_SOLID_BREP ( 'Stock-MAS-696-1', #18843 ) ;
#6180 = ORIENTED_EDGE ( 'NONE', *, *, #15811, .F. ) ;
#6181 = CARTESIAN_POINT ( 'NONE',  ( -15.21174975910705207, -51.61873716947361856, 68.25000000000000000 ) ) ;
#6182 = FACE_OUTER_BOUND ( 'NONE', #6749, .T. ) ;
#6183 = DIRECTION ( 'NONE',  ( 1.000000000000000000, 0.000000000000000000, 0.000000000000000000 ) ) ;
#6184 = LINE ( 'NONE', #12967, #12462 ) ;
#6185 = CARTESIAN_POINT ( 'NONE',  ( -3.985331397971318079, 42.46645089659917716, 69.50000000000000000 ) ) ;
#6186 = AXIS2_PLACEMENT_3D ( 'NONE', #14307, #15972, #3593 ) ;
#6187 = DIRECTION ( 'NONE',  ( 0.000000000000000000, 1.000000000000000000, 0.000000000000000000 ) ) ;
#6188 = VECTOR ( 'NONE', #13365, 1000.000000000000000 ) ;
#6189 = LINE ( 'NONE', #2689, #21534 ) ;
#6190 = SPHERICAL_SURFACE ( 'NONE', #14442, 0.5000000000000000000 ) ;
#6191 = ADVANCED_FACE ( 'NONE', ( #1614 ), #21462, .T. ) ;
#6192 = ORIENTED_EDGE ( 'NONE', *, *, #11473, .T. ) ;
#6193 = DIRECTION ( 'NONE',  ( 1.000000000000000000, 1.334402673828314029E-15, 0.000000000000000000 ) ) ;
#6194 = CARTESIAN_POINT ( 'NONE',  ( 1.824728116533979261, 42.36054587065083155, 31.70876104995653932 ) ) ;
#6195 = ORIENTED_EDGE ( 'NONE', *, *, #6257, .T. ) ;
#6196 = ORIENTED_EDGE ( 'NONE', *, *, #13195, .T. ) ;
#6197 = CARTESIAN_POINT ( 'NONE',  ( -28.87540678000427619, 6.494748934539263274, 13.50000000000000000 ) ) ;
#6198 = VECTOR ( 'NONE', #18604, 1000.000000000000000 ) ;
#6199 =( LENGTH_UNIT ( ) NAMED_UNIT ( * ) SI_UNIT ( .MILLI., .METRE. ) );
#6200 = FACE_OUTER_BOUND ( 'NONE', #3569, .T. ) ;
#6201 = ORIENTED_EDGE ( 'NONE', *, *, #3687, .T. ) ;
#6202 = DIRECTION ( 'NONE',  ( 0.000000000000000000, 0.000000000000000000, 1.000000000000000000 ) ) ;
#6203 = LINE ( 'NONE', #10998, #1295 ) ;
#6204 = ORIENTED_EDGE ( 'NONE', *, *, #22079, .T. ) ;
#6205 = CARTESIAN_POINT ( 'NONE',  ( 17.92752199202934094, -38.74634676501045760, 13.79999999999999893 ) ) ;
#6206 = DIRECTION ( 'NONE',  ( -0.000000000000000000, -1.000000000000000000, -0.000000000000000000 ) ) ;
#6207 = DIRECTION ( 'NONE',  ( -1.000000000000000000, 0.000000000000000000, 0.000000000000000000 ) ) ;
#6208 = DIRECTION ( 'NONE',  ( 4.336808689941893885E-15, 0.000000000000000000, 1.000000000000000000 ) ) ;
#6209 = EDGE_CURVE ( 'NONE', #15983, #10300, #5104, .T. ) ;
#6210 = VERTEX_POINT ( 'NONE', #3081 ) ;
#6211 = CARTESIAN_POINT ( 'NONE',  ( -10.22290649399594642, 41.92645089659918511, 68.06527860057354928 ) ) ;
#6212 = LINE ( 'NONE', #16030, #8783 ) ;
#6213 = EDGE_CURVE ( 'NONE', #15018, #20326, #6467, .T. ) ;
#6214 = ORIENTED_EDGE ( 'NONE', *, *, #10991, .F. ) ;
#6215 = EDGE_LOOP ( 'NONE', ( #11220, #5859, #19189, #11602, #9138, #6750 ) ) ;
#6216 = ORIENTED_EDGE ( 'NONE', *, *, #1223, .F. ) ;
#6217 = CARTESIAN_POINT ( 'NONE',  ( 15.13073201445138949, 52.10286008774956201, 13.87500000000000178 ) ) ;
#6218 = CARTESIAN_POINT ( 'NONE',  ( 1.774728116533979438, 42.36054587065083155, 51.70876104995653577 ) ) ;
#6219 = VERTEX_POINT ( 'NONE', #11906 ) ;
#6220 = CARTESIAN_POINT ( 'NONE',  ( 25.37540678000427263, -67.24634676501045760, 13.50000000000000000 ) ) ;
#6221 = ORIENTED_EDGE ( 'NONE', *, *, #18596, .F. ) ;
#6222 =( GEOMETRIC_REPRESENTATION_CONTEXT ( 3 ) GLOBAL_UNCERTAINTY_ASSIGNED_CONTEXT ( ( #5386 ) ) GLOBAL_UNIT_ASSIGNED_CONTEXT ( ( #14782, #4731, #4619 ) ) REPRESENTATION_CONTEXT ( 'NONE', 'WORKASPACE' ) );
#6223 = CARTESIAN_POINT ( 'NONE',  ( -9.641460742840918030, 32.61873716947361856, 68.00000000000000000 ) ) ;
#6224 = DIRECTION ( 'NONE',  ( 1.000000000000000000, 0.000000000000000000, 0.000000000000000000 ) ) ;
#6225 = EDGE_CURVE ( 'NONE', #22131, #12877, #8134, .T. ) ;
#6226 = DIRECTION ( 'NONE',  ( -1.000000000000000000, -0.000000000000000000, -0.000000000000000000 ) ) ;
#6227 = CARTESIAN_POINT ( 'NONE',  ( -1.724728116533986721, 43.26054587065083012, 27.80876104995653719 ) ) ;
#6228 = DIRECTION ( 'NONE',  ( 0.000000000000000000, 0.000000000000000000, -1.000000000000000000 ) ) ;
#6229 = DIRECTION ( 'NONE',  ( 0.000000000000000000, 0.000000000000000000, 1.000000000000000000 ) ) ;
#6230 = ORIENTED_EDGE ( 'NONE', *, *, #14189, .F. ) ;
#6231 = FACE_OUTER_BOUND ( 'NONE', #11768, .T. ) ;
#6232 = CARTESIAN_POINT ( 'NONE',  ( -14.66174975910705136, 42.11054587065083155, 13.50000000000000000 ) ) ;
#6233 = AXIS2_PLACEMENT_3D ( 'NONE', #3899, #15733, #19427 ) ;
#6234 = DIRECTION ( 'NONE',  ( 0.000000000000000000, -1.000000000000000000, 0.000000000000000000 ) ) ;
#6235 = CYLINDRICAL_SURFACE ( 'NONE', #21607, 0.3000000000000016542 ) ;
#6236 = CYLINDRICAL_SURFACE ( 'NONE', #3315, 4.193574995607837863 ) ;
#6237 = VERTEX_POINT ( 'NONE', #6679 ) ;
#6238 = DIRECTION ( 'NONE',  ( 0.000000000000000000, 1.000000000000000000, 0.000000000000000000 ) ) ;
#6239 = DIRECTION ( 'NONE',  ( 1.000000000000000000, 0.000000000000000000, 0.000000000000000000 ) ) ;
#6240 = EDGE_CURVE ( 'NONE', #17330, #1152, #5590, .T. ) ;
#6241 = EDGE_CURVE ( 'NONE', #3604, #2394, #20221, .T. ) ;
#6242 = ORIENTED_EDGE ( 'NONE', *, *, #12169, .T. ) ;
#6243 = DIRECTION ( 'NONE',  ( 0.000000000000000000, -1.000000000000000000, 0.000000000000000000 ) ) ;
#6244 = AXIS2_PLACEMENT_3D ( 'NONE', #13860, #7280, #5729 ) ;
#6245 = EDGE_CURVE ( 'NONE', #12241, #17488, #4663, .T. ) ;
#6246 = CARTESIAN_POINT ( 'NONE',  ( 3.627054932750481964, 33.43424481021354921, 42.50000000000000000 ) ) ;
#6247 = ORIENTED_EDGE ( 'NONE', *, *, #3989, .F. ) ;
#6248 = ORIENTED_EDGE ( 'NONE', *, *, #1200, .F. ) ;
#6249 = VERTEX_POINT ( 'NONE', #6577 ) ;
#6250 = LINE ( 'NONE', #11374, #17051 ) ;
#6252 = EDGE_CURVE ( 'NONE', #11265, #1826, #14125, .T. ) ;
#6251 = CARTESIAN_POINT ( 'NONE',  ( 31.69597781366222122, 56.94165929845684104, 68.75000000000000000 ) ) ;
#6253 = DIRECTION ( 'NONE',  ( 0.000000000000000000, 0.000000000000000000, 1.000000000000000000 ) ) ;
#6254 = ORIENTED_EDGE ( 'NONE', *, *, #5973, .T. ) ;
#6255 = ORIENTED_EDGE ( 'NONE', *, *, #20528, .F. ) ;
#6256 = CARTESIAN_POINT ( 'NONE',  ( 34.39999999999998437, 85.00000000000000000, 79.39999999999999147 ) ) ;
#6257 = EDGE_CURVE ( 'NONE', #1350, #18032, #13042, .T. ) ;
#6258 = CARTESIAN_POINT ( 'NONE',  ( 1.824728116533979705, 43.31054587065082728, 45.66679706732590205 ) ) ;
#6259 = DIRECTION ( 'NONE',  ( -1.000000000000000000, 0.000000000000000000, 0.000000000000000000 ) ) ;
#6260 = DIRECTION ( 'NONE',  ( -0.000000000000000000, -1.000000000000000000, -0.000000000000000000 ) ) ;
#6261 = CIRCLE ( 'NONE', #16589, 1.000000000000000888 ) ;
#6262 = DIRECTION ( 'NONE',  ( 0.000000000000000000, -1.000000000000000000, 0.000000000000000000 ) ) ;
#6263 = CYLINDRICAL_SURFACE ( 'NONE', #2454, 0.2999999999999947153 ) ;
#6264 = CARTESIAN_POINT ( 'NONE',  ( 27.77120804565220169, -2.094189496455408861, 0.2999999999999947153 ) ) ;
#6265 = CARTESIAN_POINT ( 'NONE',  ( 29.37540678000427619, -5.299999999999999822, 7.200000000000000178 ) ) ;
#6266 = VERTEX_POINT ( 'NONE', #3203 ) ;
#6267 = DIRECTION ( 'NONE',  ( -0.000000000000000000, -0.000000000000000000, -1.000000000000000000 ) ) ;
#6268 = CARTESIAN_POINT ( 'NONE',  ( -1.724728116533986721, 43.26054587065083012, 51.80876104995653719 ) ) ;
#6269 = EDGE_CURVE ( 'NONE', #8250, #2324, #8241, .T. ) ;
#6270 = FACE_OUTER_BOUND ( 'NONE', #4623, .T. ) ;
#6271 = ORIENTED_EDGE ( 'NONE', *, *, #21179, .F. ) ;
#6272 = ADVANCED_FACE ( 'NONE', ( #16729 ), #20203, .F. ) ;
#6273 = CARTESIAN_POINT ( 'NONE',  ( 29.17540678000427690, 0.000000000000000000, 7.500000000000000000 ) ) ;
#6274 = ORIENTED_EDGE ( 'NONE', *, *, #15265, .T. ) ;
#6275 = ORIENTED_EDGE ( 'NONE', *, *, #9102, .F. ) ;
#6276 = CARTESIAN_POINT ( 'NONE',  ( 1.724728116533979616, 43.31054587065082728, 41.76679706732590347 ) ) ;
#6277 = SHAPE_REPRESENTATION ( 'Glass Cover', ( #17493 ), #19794 ) ;
#6278 = AXIS2_PLACEMENT_3D ( 'NONE', #11062, #9389, #6163 ) ;
#6279 = DIRECTION ( 'NONE',  ( 1.000000000000000000, 0.000000000000000000, 0.000000000000000000 ) ) ;
#6280 = ADVANCED_FACE ( 'NONE', ( #4771 ), #10135, .T. ) ;
#6281 = CARTESIAN_POINT ( 'NONE',  ( 0.000000000000000000, -51.61873716947361856, 68.50000000000000000 ) ) ;
#6282 = DIRECTION ( 'NONE',  ( 0.000000000000000000, 1.000000000000000000, 0.000000000000000000 ) ) ;
#6283 = EDGE_CURVE ( 'NONE', #1945, #4392, #3058, .T. ) ;
#6284 = CARTESIAN_POINT ( 'NONE',  ( -1.774728116533986766, 42.36054587065083155, 41.66679706732590915 ) ) ;
#6285 = CIRCLE ( 'NONE', #1980, 0.2999999999999999334 ) ;
#6286 = CIRCLE ( 'NONE', #11977, 0.2500000000000002220 ) ;
#6287 = CARTESIAN_POINT ( 'NONE',  ( -15.95292532278785913, -32.11873716947361856, 42.50000000000000711 ) ) ;
#6288 = DIRECTION ( 'NONE',  ( 1.000000000000000000, 0.000000000000000000, 0.000000000000000000 ) ) ;
#6289 = DIRECTION ( 'NONE',  ( -0.000000000000000000, -0.000000000000000000, -1.000000000000000000 ) ) ;
#6290 = DIRECTION ( 'NONE',  ( -1.000000000000000000, 0.000000000000000000, 0.000000000000000000 ) ) ;
#6291 = ADVANCED_FACE ( 'NONE', ( #20322 ), #6911, .T. ) ;
#6292 = EDGE_LOOP ( 'NONE', ( #21579, #7424, #15019, #5174 ) ) ;
#6293 = ORIENTED_EDGE ( 'NONE', *, *, #5067, .F. ) ;
#6294 = CARTESIAN_POINT ( 'NONE',  ( -29.13662752439705272, 0.000000000000000000, 7.500000000000000000 ) ) ;
#6295 = DIRECTION ( 'NONE',  ( -4.336808689941893885E-15, 0.000000000000000000, 1.000000000000000000 ) ) ;
#6296 = ORIENTED_EDGE ( 'NONE', *, *, #14704, .T. ) ;
#6297 = VECTOR ( 'NONE', #20281, 1000.000000000000000 ) ;
#6298 = VERTEX_POINT ( 'NONE', #18519 ) ;
#6299 = DIRECTION ( 'NONE',  ( 0.000000000000000000, 1.000000000000000000, 0.000000000000000000 ) ) ;
#6300 =( NAMED_UNIT ( * ) PLANE_ANGLE_UNIT ( ) SI_UNIT ( $, .RADIAN. ) );
#6301 = ORIENTED_EDGE ( 'NONE', *, *, #18351, .F. ) ;
#6302 = AXIS2_PLACEMENT_3D ( 'NONE', #12194, #343, #20840 ) ;
#6303 = AXIS2_PLACEMENT_3D ( 'NONE', #11106, #16026, #19402 ) ;
#6304 = VECTOR ( 'NONE', #5695, 1000.000000000000000 ) ;
#6305 = VERTEX_POINT ( 'NONE', #16945 ) ;
#6306 = ORIENTED_EDGE ( 'NONE', *, *, #16978, .F. ) ;
#6307 = ORIENTED_EDGE ( 'NONE', *, *, #20945, .T. ) ;
#6308 = ADVANCED_FACE ( 'NONE', ( #15387 ), #60, .T. ) ;
#6309 = CARTESIAN_POINT ( 'NONE',  ( -23.02398829872513986, 5.683640910026983128, 42.50000000000000000 ) ) ;
#6310 = EDGE_CURVE ( 'NONE', #1165, #6037, #11474, .T. ) ;
#6311 = AXIS2_PLACEMENT_3D ( 'NONE', #21773, #10123, #8116 ) ;
#6312 = DIRECTION ( 'NONE',  ( 1.000000000000000000, 0.000000000000000000, 0.000000000000000000 ) ) ;
#6313 = AXIS2_PLACEMENT_3D ( 'NONE', #20148, #13645, #20489 ) ;
#6314 = ORIENTED_EDGE ( 'NONE', *, *, #13744, .T. ) ;
#6315 = FILL_AREA_STYLE_COLOUR ( '', #6095 ) ;
#6316 = FACE_OUTER_BOUND ( 'NONE', #4553, .T. ) ;
#6317 = CARTESIAN_POINT ( 'NONE',  ( 26.56227312273159313, -9.958410664601842655, 13.79999999999999893 ) ) ;
#6318 = CARTESIAN_POINT ( 'NONE',  ( -23.04906723162513416, 2.296088124452694501, 13.26119099173120652 ) ) ;
#6319 = CIRCLE ( 'NONE', #20956, 2.000000000000001776 ) ;
#6320 = ORIENTED_EDGE ( 'NONE', *, *, #12933, .F. ) ;
#6321 = LINE ( 'NONE', #11331, #1860 ) ;
#6322 = ORIENTED_EDGE ( 'NONE', *, *, #20217, .T. ) ;
#6323 = ORIENTED_EDGE ( 'NONE', *, *, #96, .F. ) ;
#6324 = ORIENTED_EDGE ( 'NONE', *, *, #18554, .F. ) ;
#6325 = CARTESIAN_POINT ( 'NONE',  ( 14.96174975910705918, 51.76873716947361714, 13.79999999999999716 ) ) ;
#6326 = CARTESIAN_POINT ( 'NONE',  ( 31.69597781366222122, 58.94165929845684104, 68.75000000000000000 ) ) ;
#6327 = ORIENTED_EDGE ( 'NONE', *, *, #211, .F. ) ;
#6328 = AXIS2_PLACEMENT_3D ( 'NONE', #2409, #828, #11024 ) ;
#6329 = EDGE_CURVE ( 'NONE', #2605, #12981, #4851, .T. ) ;
#6330 = VECTOR ( 'NONE', #9042, 1000.000000000000000 ) ;
#6331 = CARTESIAN_POINT ( 'NONE',  ( -1.724728116533986721, 42.36054587065083155, 35.75876104995654003 ) ) ;
#6332 = VECTOR ( 'NONE', #21839, 1000.000000000000000 ) ;
#6333 = VERTEX_POINT ( 'NONE', #267 ) ;
#6334 = LINE ( 'NONE', #4652, #17902 ) ;
#6335 = AXIS2_PLACEMENT_3D ( 'NONE', #8304, #3153, #8524 ) ;
#6336 = DIRECTION ( 'NONE',  ( -0.000000000000000000, 0.000000000000000000, 1.000000000000000000 ) ) ;
#6337 = ADVANCED_FACE ( 'NONE', ( #5338 ), #15487, .T. ) ;
#6338 = EDGE_CURVE ( 'NONE', #1535, #18691, #7121, .T. ) ;
#6339 = CARTESIAN_POINT ( 'NONE',  ( 23.02398829872513986, -2.192334671524723166, 13.33121981694520564 ) ) ;
#6340 = DIRECTION ( 'NONE',  ( -0.000000000000000000, -1.000000000000000000, -0.000000000000000000 ) ) ;
#6341 = EDGE_LOOP ( 'NONE', ( #333, #8992, #9202, #19167 ) ) ;
#6342 = CARTESIAN_POINT ( 'NONE',  ( -33.20000000000000284, -85.00000000000000000, 1.800000000000000266 ) ) ;
#6343 = CARTESIAN_POINT ( 'NONE',  ( 1.724728116533979616, 43.26054587065083012, 47.75876104995653293 ) ) ;
#6344 = CIRCLE ( 'NONE', #15250, 0.2999999999999999889 ) ;
#6345 = LINE ( 'NONE', #14479, #16195 ) ;
#6346 = CARTESIAN_POINT ( 'NONE',  ( -1.824728116533986810, 43.26054587065083012, 39.80876104995653719 ) ) ;
#6347 = ORIENTED_EDGE ( 'NONE', *, *, #1574, .T. ) ;
#6348 = AXIS2_PLACEMENT_3D ( 'NONE', #8062, #7853, #19933 ) ;
#6349 = VECTOR ( 'NONE', #20389, 1000.000000000000000 ) ;
#6350 = DIRECTION ( 'NONE',  ( -0.000000000000000000, -0.000000000000000000, -1.000000000000000000 ) ) ;
#6351 = DIRECTION ( 'NONE',  ( -0.000000000000000000, -0.000000000000000000, 1.000000000000000000 ) ) ;
#6352 = VECTOR ( 'NONE', #18662, 1000.000000000000000 ) ;
#6353 = ORIENTED_EDGE ( 'NONE', *, *, #15726, .T. ) ;
#6354 = DIRECTION ( 'NONE',  ( 0.000000000000000000, 1.000000000000000000, -0.000000000000000000 ) ) ;
#6355 = AXIS2_PLACEMENT_3D ( 'NONE', #9233, #16247, #11118 ) ;
#6356 = LINE ( 'NONE', #3316, #17370 ) ;
#6357 = ORIENTED_EDGE ( 'NONE', *, *, #12013, .F. ) ;
#6358 = VERTEX_POINT ( 'NONE', #2276 ) ;
#6359 = CIRCLE ( 'NONE', #8493, 0.5000000000000004441 ) ;
#6360 = ORIENTED_EDGE ( 'NONE', *, *, #5117, .T. ) ;
#6361 = CARTESIAN_POINT ( 'NONE',  ( 0.000000000000000000, -68.70000000000001705, 0.2999999999999947153 ) ) ;
#6362 = EDGE_CURVE ( 'NONE', #16887, #3080, #12451, .T. ) ;
#6363 = DIRECTION ( 'NONE',  ( 0.000000000000000000, 0.000000000000000000, 1.000000000000000000 ) ) ;
#6364 = EDGE_LOOP ( 'NONE', ( #9376, #10754, #7384, #12131 ) ) ;
#6365 = VERTEX_POINT ( 'NONE', #3744 ) ;
#6366 = CIRCLE ( 'NONE', #17774, 0.2999999999999999334 ) ;
#6367 = DIRECTION ( 'NONE',  ( -0.000000000000000000, -0.000000000000000000, 1.000000000000000000 ) ) ;
#6368 = AXIS2_PLACEMENT_3D ( 'NONE', #1987, #5492, #315 ) ;
#6369 = AXIS2_PLACEMENT_3D ( 'NONE', #14755, #2908, #8173 ) ;
#6370 = EDGE_CURVE ( 'NONE', #21952, #12463, #904, .T. ) ;
#6371 = DIRECTION ( 'NONE',  ( -1.000000000000000000, 0.000000000000000000, 0.000000000000000000 ) ) ;
#6372 = LINE ( 'NONE', #19900, #17063 ) ;
#6373 = EDGE_CURVE ( 'NONE', #12411, #12755, #11276, .T. ) ;
#6374 = DIRECTION ( 'NONE',  ( 1.000000000000000000, 0.000000000000000000, 0.000000000000000000 ) ) ;
#6375 = DIRECTION ( 'NONE',  ( -0.000000000000000000, -0.000000000000000000, -1.000000000000000000 ) ) ;
#6376 = AXIS2_PLACEMENT_3D ( 'NONE', #13345, #13577, #3515 ) ;
#6377 = DIRECTION ( 'NONE',  ( 1.000000000000000000, 0.000000000000000000, 0.000000000000000000 ) ) ;
#6378 = VERTEX_POINT ( 'NONE', #1940 ) ;
#6379 = AXIS2_PLACEMENT_3D ( 'NONE', #2181, #13809, #17285 ) ;
#6380 = DIRECTION ( 'NONE',  ( 0.000000000000000000, 1.000000000000000000, 0.000000000000000000 ) ) ;
#6381 = CARTESIAN_POINT ( 'NONE',  ( 25.37540678000427263, -69.04634676501045476, 3.799999999999999822 ) ) ;
#6382 = CARTESIAN_POINT ( 'NONE',  ( -1.824728116533986810, 43.31054587065082728, 41.66679706732590915 ) ) ;
#6383 = VERTEX_POINT ( 'NONE', #3535 ) ;
#6384 = DIRECTION ( 'NONE',  ( 0.000000000000000000, 0.000000000000000000, -1.000000000000000000 ) ) ;
#6385 = VECTOR ( 'NONE', #19758, 1000.000000000000000 ) ;
#6386 = VECTOR ( 'NONE', #309, 1000.000000000000000 ) ;
#6387 = ORIENTED_EDGE ( 'NONE', *, *, #8772, .F. ) ;
#6388 = DIRECTION ( 'NONE',  ( 1.000000000000000000, 0.000000000000000000, 0.000000000000000000 ) ) ;
#6389 = EDGE_CURVE ( 'NONE', #3240, #5820, #17502, .T. ) ;
#6390 = DIRECTION ( 'NONE',  ( 0.000000000000000000, 0.000000000000000000, 1.000000000000000000 ) ) ;
#6391 = VERTEX_POINT ( 'NONE', #10366 ) ;
#6392 = TOROIDAL_SURFACE ( 'NONE', #20679, 0.05000000000000000278, 0.05000000000000000278 ) ;
#6393 = EDGE_LOOP ( 'NONE', ( #10033, #4414, #14064, #242 ) ) ;
#6394 = AXIS2_PLACEMENT_3D ( 'NONE', #15112, #1462, #6537 ) ;
#6395 = CARTESIAN_POINT ( 'NONE',  ( 3.127054932750481964, 32.11873716947361856, 109.6002446535588319 ) ) ;
#6396 = VECTOR ( 'NONE', #13935, 1000.000000000000000 ) ;
#6397 = VERTEX_POINT ( 'NONE', #12012 ) ;
#6398 = EDGE_CURVE ( 'NONE', #14518, #1148, #12125, .T. ) ;
#6399 = CARTESIAN_POINT ( 'NONE',  ( 1.824728116533979261, 43.31054587065082728, 47.70876104995654288 ) ) ;
#6400 = ORIENTED_EDGE ( 'NONE', *, *, #21195, .F. ) ;
#6401 = DIRECTION ( 'NONE',  ( 1.000000000000000000, 0.000000000000000000, 0.000000000000000000 ) ) ;
#6402 = EDGE_CURVE ( 'NONE', #5867, #9603, #13693, .T. ) ;
#6403 = AXIS2_PLACEMENT_3D ( 'NONE', #21969, #13444, #3170 ) ;
#6404 = EDGE_CURVE ( 'NONE', #20447, #14241, #11976, .T. ) ;
#6405 = DIRECTION ( 'NONE',  ( 0.000000000000000000, 0.000000000000000000, 1.000000000000000000 ) ) ;
#6406 = LINE ( 'NONE', #13310, #17026 ) ;
#6407 = AXIS2_PLACEMENT_3D ( 'NONE', #180, #10594, #7034 ) ;
#6408 = AXIS2_PLACEMENT_3D ( 'NONE', #10228, #14916, #16706 ) ;
#6409 = CARTESIAN_POINT ( 'NONE',  ( -1.774728116533986766, 42.31054587065082728, 0.000000000000000000 ) ) ;
#6410 = DIRECTION ( 'NONE',  ( 0.000000000000000000, 0.000000000000000000, 1.000000000000000000 ) ) ;
#6411 = VECTOR ( 'NONE', #16437, 1000.000000000000000 ) ;
#6412 = CARTESIAN_POINT ( 'NONE',  ( 30.49999999999999645, 69.70000000000000284, 1.200000000000003064 ) ) ;
#6413 = CARTESIAN_POINT ( 'NONE',  ( -1.724728116533986721, 42.36054587065083155, 37.66679706732590915 ) ) ;
#6414 = CARTESIAN_POINT ( 'NONE',  ( 28.87540678000427619, -6.494748934539263274, 7.799999999999999822 ) ) ;
#6415 = LINE ( 'NONE', #1225, #10616 ) ;
#6416 = EDGE_LOOP ( 'NONE', ( #16145, #16205, #21599, #4998 ) ) ;
#6417 = CYLINDRICAL_SURFACE ( 'NONE', #16300, 0.1000000000000028644 ) ;
#6418 = CIRCLE ( 'NONE', #18914, 0.5000000000000004441 ) ;
#6419 = CIRCLE ( 'NONE', #10678, 1.999999999999991340 ) ;
#6420 = DIRECTION ( 'NONE',  ( 1.000000000000000000, 0.000000000000000000, 6.123233995736764803E-17 ) ) ;
#6421 = ORIENTED_EDGE ( 'NONE', *, *, #169, .T. ) ;
#6422 = ORIENTED_EDGE ( 'NONE', *, *, #1699, .T. ) ;
#6423 = CARTESIAN_POINT ( 'NONE',  ( 1.774728116533979660, 43.26054587065083012, 43.80876104995653719 ) ) ;
#6424 = EDGE_CURVE ( 'NONE', #4947, #6383, #5932, .T. ) ;
#6425 = UNCERTAINTY_MEASURE_WITH_UNIT (LENGTH_MEASURE( 1.000000000000000082E-05 ), #8577, 'distance_accuracy_value', 'NONE');
#6426 = AXIS2_PLACEMENT_3D ( 'NONE', #20101, #1393, #13145 ) ;
#6427 = DIRECTION ( 'NONE',  ( -1.000000000000000000, 1.094601647044990554E-16, 0.000000000000000000 ) ) ;
#6428 = ORIENTED_EDGE ( 'NONE', *, *, #20299, .F. ) ;
#6429 = VECTOR ( 'NONE', #7064, 999.9999999999998863 ) ;
#6430 = ORIENTED_EDGE ( 'NONE', *, *, #2626, .F. ) ;
#6431 = EDGE_LOOP ( 'NONE', ( #20275, #7268, #6387, #3957 ) ) ;
#6432 = EDGE_CURVE ( 'NONE', #6397, #8329, #19147, .T. ) ;
#6433 = CARTESIAN_POINT ( 'NONE',  ( 15.04770344846787822, -51.92604205163220854, 13.50000000000000000 ) ) ;
#6434 = CARTESIAN_POINT ( 'NONE',  ( -25.37540678000427263, -63.74634676501045050, 13.50000000000000000 ) ) ;
#6435 = ORIENTED_EDGE ( 'NONE', *, *, #6830, .T. ) ;
#6436 = CARTESIAN_POINT ( 'NONE',  ( 29.13662752439705272, 0.000000000000000000, 7.500000000000000000 ) ) ;
#6437 = DIRECTION ( 'NONE',  ( 1.000000000000000000, 0.000000000000000000, 0.000000000000000000 ) ) ;
#6438 = CIRCLE ( 'NONE', #2844, 0.2999999999999999334 ) ;
#6439 = CARTESIAN_POINT ( 'NONE',  ( -20.10144383993102934, 42.46645089659918426, 68.50000000000000000 ) ) ;
#6440 = CARTESIAN_POINT ( 'NONE',  ( -28.87540678000427619, 6.494748934539263274, 7.799999999999999822 ) ) ;
#6441 = CARTESIAN_POINT ( 'NONE',  ( -21.92816239687475743, 42.46645089659918426, 68.50000000000000000 ) ) ;
#6442 = VERTEX_POINT ( 'NONE', #18976 ) ;
#6443 = ORIENTED_EDGE ( 'NONE', *, *, #1158, .T. ) ;
#6444 = VERTEX_POINT ( 'NONE', #20657 ) ;
#6445 = DIRECTION ( 'NONE',  ( -1.000000000000000000, 0.000000000000000000, 0.000000000000000000 ) ) ;
#6447 = EDGE_CURVE ( 'NONE', #8429, #2851, #3644, .T. ) ;
#6446 = CARTESIAN_POINT ( 'NONE',  ( -29.50000000000002132, -2.473451120191013430, 0.2999999999999947153 ) ) ;
#6448 = EDGE_LOOP ( 'NONE', ( #3043, #16856, #17133, #2064 ) ) ;
#6449 = ADVANCED_FACE ( 'NONE', ( #13916 ), #10687, .T. ) ;
#6450 = FACE_OUTER_BOUND ( 'NONE', #15903, .T. ) ;
#6451 = TOROIDAL_SURFACE ( 'NONE', #18946, 1.750000000000000000, 0.2500000000000000000 ) ;
#6452 = CIRCLE ( 'NONE', #11441, 4.051418481279135619 ) ;
#6453 = CIRCLE ( 'NONE', #15694, 0.2999999999999999334 ) ;
#6454 = PRODUCT ( 'Cross Recess Screw', 'Cross Recess Screw', '', ( #5397 ) ) ;
#6455 = VERTEX_POINT ( 'NONE', #9107 ) ;
#6456 = CARTESIAN_POINT ( 'NONE',  ( -29.13662752439705272, 0.000000000000000000, 0.3000000000000016542 ) ) ;
#6457 = CARTESIAN_POINT ( 'NONE',  ( -1.774728116533986766, 42.36054587065083155, 43.80876104995653719 ) ) ;
#6458 = DIRECTION ( 'NONE',  ( 0.000000000000000000, -1.000000000000000000, 0.000000000000000000 ) ) ;
#6459 = DIRECTION ( 'NONE',  ( 1.000000000000000000, -0.000000000000000000, 0.000000000000000000 ) ) ;
#6460 = VERTEX_POINT ( 'NONE', #375 ) ;
#6461 = FACE_OUTER_BOUND ( 'NONE', #8348, .T. ) ;
#6462 = DIRECTION ( 'NONE',  ( -0.000000000000000000, -1.000000000000000000, -0.000000000000000000 ) ) ;
#6463 = CYLINDRICAL_SURFACE ( 'NONE', #13355, 0.05000000000000143219 ) ;
#6464 = DIRECTION ( 'NONE',  ( 1.000000000000000000, 0.000000000000000000, -1.224646799147353207E-16 ) ) ;
#6465 = ORIENTED_EDGE ( 'NONE', *, *, #6524, .T. ) ;
#6466 = EDGE_CURVE ( 'NONE', #19513, #18311, #15909, .T. ) ;
#6467 = LINE ( 'NONE', #9914, #7713 ) ;
#6468 = EDGE_CURVE ( 'NONE', #6365, #11863, #8430, .T. ) ;
#6469 = CARTESIAN_POINT ( 'NONE',  ( 31.50000000000002132, 71.70000000000001705, 1.800000000000000044 ) ) ;
#6470 = VECTOR ( 'NONE', #4264, 1000.000000000000000 ) ;
#6471 = ORIENTED_EDGE ( 'NONE', *, *, #10260, .F. ) ;
#6472 = AXIS2_PLACEMENT_3D ( 'NONE', #17027, #1702, #8214 ) ;
#6473 = DIRECTION ( 'NONE',  ( 0.000000000000000000, 1.000000000000000000, 0.000000000000000000 ) ) ;
#6474 = CARTESIAN_POINT ( 'NONE',  ( 25.37540678000426908, 38.74634676501045760, 13.79999999999999893 ) ) ;
#6475 = ORIENTED_EDGE ( 'NONE', *, *, #9918, .F. ) ;
#6476 = ORIENTED_EDGE ( 'NONE', *, *, #9768, .T. ) ;
#6477 = ORIENTED_EDGE ( 'NONE', *, *, #18269, .F. ) ;
#6478 = CARTESIAN_POINT ( 'NONE',  ( 15.21174975910705918, -52.39333383871510108, 13.50000000000000000 ) ) ;
#6479 = LINE ( 'NONE', #16956, #15985 ) ;
#6480 = EDGE_CURVE ( 'NONE', #15917, #10124, #918, .T. ) ;
#6481 = DIRECTION ( 'NONE',  ( 1.000000000000000000, -0.000000000000000000, -0.000000000000000000 ) ) ;
#6482 = EDGE_LOOP ( 'NONE', ( #633, #2514, #15506, #7506 ) ) ;
#6483 = ORIENTED_EDGE ( 'NONE', *, *, #3199, .F. ) ;
#6484 = DIRECTION ( 'NONE',  ( 0.000000000000000000, 0.000000000000000000, 1.000000000000000000 ) ) ;
#6485 = CIRCLE ( 'NONE', #1814, 0.6999999999999992895 ) ;
#6486 = DIRECTION ( 'NONE',  ( -1.000000000000000000, -0.000000000000000000, -4.336808689942194441E-15 ) ) ;
#6487 = CARTESIAN_POINT ( 'NONE',  ( -23.02398829872513986, -2.928742984578568187, 13.54178985689086190 ) ) ;
#6488 = AXIS2_PLACEMENT_3D ( 'NONE', #13669, #18828, #3501 ) ;
#6489 = CARTESIAN_POINT ( 'NONE',  ( 14.96174975910707161, 51.86873716947361856, 68.00000000000000000 ) ) ;
#6490 = CARTESIAN_POINT ( 'NONE',  ( 0.000000000000000000, -69.00000000000000000, -150.0833101980363722 ) ) ;
#6491 = DIRECTION ( 'NONE',  ( -0.000000000000000000, 1.000000000000000000, -0.000000000000000000 ) ) ;
#6492 = CARTESIAN_POINT ( 'NONE',  ( 1.724728116533978728, 43.31054587065082728, 53.71679706732590631 ) ) ;
#6493 = EDGE_CURVE ( 'NONE', #18912, #10431, #13418, .T. ) ;
#6494 = DIRECTION ( 'NONE',  ( 0.000000000000000000, 0.000000000000000000, 1.000000000000000000 ) ) ;
#6495 = DIRECTION ( 'NONE',  ( 0.000000000000000000, 0.000000000000000000, 1.000000000000000000 ) ) ;
#6496 = ORIENTED_EDGE ( 'NONE', *, *, #19073, .T. ) ;
#6497 = CARTESIAN_POINT ( 'NONE',  ( 30.37540678000427619, -6.000000000000000000, 3.799999999999999822 ) ) ;
#6498 = VECTOR ( 'NONE', #6803, 1000.000000000000000 ) ;
#6499 = CARTESIAN_POINT ( 'NONE',  ( 3.627054932750481964, -33.43424481021354921, 42.50000000000000000 ) ) ;
#6500 = EDGE_LOOP ( 'NONE', ( #145, #5913, #3762, #12595, #20800, #5189, #21042, #17465 ) ) ;
#6501 = FACE_OUTER_BOUND ( 'NONE', #20109, .T. ) ;
#6502 = CARTESIAN_POINT ( 'NONE',  ( -34.39999999999999858, -85.00000000000000000, 0.6000000000000033085 ) ) ;
#6503 = CIRCLE ( 'NONE', #21844, 0.2999999999999999334 ) ;
#6504 = VERTEX_POINT ( 'NONE', #14688 ) ;
#6505 = EDGE_CURVE ( 'NONE', #18602, #421, #19624, .T. ) ;
#6506 = EDGE_LOOP ( 'NONE', ( #216, #14457, #482, #16653 ) ) ;
#6507 = TOROIDAL_SURFACE ( 'NONE', #12902, 0.5999999999999999778, 0.2999999999999999889 ) ;
#6508 = VERTEX_POINT ( 'NONE', #16237 ) ;
#6509 = CIRCLE ( 'NONE', #19007, 5.193574995607837863 ) ;
#6510 = AXIS2_PLACEMENT_3D ( 'NONE', #10215, #17031, #8548 ) ;
#6511 = FACE_OUTER_BOUND ( 'NONE', #18694, .T. ) ;
#6512 = VERTEX_POINT ( 'NONE', #4074 ) ;
#6513 = FACE_OUTER_BOUND ( 'NONE', #12409, .T. ) ;
#6514 = CIRCLE ( 'NONE', #5810, 3.017785046117004377 ) ;
#6515 = CARTESIAN_POINT ( 'NONE',  ( 29.13662752439705272, 5.299999999999999822, 7.200000000000000178 ) ) ;
#6516 = DIRECTION ( 'NONE',  ( 1.000000000000000000, 0.000000000000000000, 0.000000000000000000 ) ) ;
#6517 = EDGE_CURVE ( 'NONE', #10408, #10275, #1255, .T. ) ;
#6518 = CARTESIAN_POINT ( 'NONE',  ( 23.14059574490499571, 2.755557770589327049, 13.42404417222474322 ) ) ;
#6519 = DIRECTION ( 'NONE',  ( -0.9823853469773031755, 0.1868663427273193067, 0.000000000000000000 ) ) ;
#6520 = CARTESIAN_POINT ( 'NONE',  ( -1.724728116533986721, 43.31054587065082728, 53.71679706732590631 ) ) ;
#6521 = DIRECTION ( 'NONE',  ( -1.224646799147353207E-16, -0.000000000000000000, -1.000000000000000000 ) ) ;
#6522 = CARTESIAN_POINT ( 'NONE',  ( 29.17540678000427690, -63.74634676501045050, 7.799999999999999822 ) ) ;
#6523 = AXIS2_PLACEMENT_3D ( 'NONE', #7030, #1960, #15611 ) ;
#6524 = EDGE_CURVE ( 'NONE', #15631, #15087, #21311, .T. ) ;
#6525 = VERTEX_POINT ( 'NONE', #5986 ) ;
#6526 = VECTOR ( 'NONE', #18248, 1000.000000000000000 ) ;
#6527 = FACE_OUTER_BOUND ( 'NONE', #20357, .T. ) ;
#6528 = ORIENTED_EDGE ( 'NONE', *, *, #21307, .F. ) ;
#6529 = CARTESIAN_POINT ( 'NONE',  ( 29.50000000000002132, 2.512390033608338236, 1.500000000000000000 ) ) ;
#6530 = AXIS2_PLACEMENT_3D ( 'NONE', #16099, #1113, #13074 ) ;
#6531 = VECTOR ( 'NONE', #2328, 1000.000000000000000 ) ;
#6532 = EDGE_CURVE ( 'NONE', #8285, #17988, #8784, .T. ) ;
#6533 = DIRECTION ( 'NONE',  ( 1.000000000000000000, 0.000000000000000000, 0.000000000000000000 ) ) ;
#6534 = EDGE_LOOP ( 'NONE', ( #1075, #14313, #7056, #11538 ) ) ;
#6535 = AXIS2_PLACEMENT_3D ( 'NONE', #10967, #21174, #11180 ) ;
#6536 = VERTEX_POINT ( 'NONE', #17936 ) ;
#6537 = DIRECTION ( 'NONE',  ( 1.000000000000000000, 0.000000000000000000, 0.000000000000000000 ) ) ;
#6538 = ADVANCED_FACE ( 'NONE', ( #12780 ), #10891, .T. ) ;
#6539 = ORIENTED_EDGE ( 'NONE', *, *, #13137, .F. ) ;
#6540 = SURFACE_STYLE_FILL_AREA ( #8204 ) ;
#6541 = ORIENTED_EDGE ( 'NONE', *, *, #18026, .F. ) ;
#6542 = ORIENTED_EDGE ( 'NONE', *, *, #701, .T. ) ;
#6543 = ORIENTED_EDGE ( 'NONE', *, *, #14223, .T. ) ;
#6544 = AXIS2_PLACEMENT_3D ( 'NONE', #2001, #209, #14190 ) ;
#6545 = EDGE_CURVE ( 'NONE', #252, #9928, #9854, .T. ) ;
#6546 = DIRECTION ( 'NONE',  ( 0.000000000000000000, 0.000000000000000000, -1.000000000000000000 ) ) ;
#6547 = AXIS2_PLACEMENT_3D ( 'NONE', #4791, #6377, #9484 ) ;
#6548 = FACE_OUTER_BOUND ( 'NONE', #1600, .T. ) ;
#6549 = ORIENTED_EDGE ( 'NONE', *, *, #20712, .F. ) ;
#6550 = DIRECTION ( 'NONE',  ( -0.000000000000000000, -0.000000000000000000, -1.000000000000000000 ) ) ;
#6551 = CARTESIAN_POINT ( 'NONE',  ( -23.20982120895258660, 3.064530420494592899, 13.47289532992770589 ) ) ;
#6552 = CARTESIAN_POINT ( 'NONE',  ( 1.824728116533979261, 42.36054587065083155, 39.70876104995653577 ) ) ;
#6553 = AXIS2_PLACEMENT_3D ( 'NONE', #19381, #17586, #13887 ) ;
#6554 = CARTESIAN_POINT ( 'NONE',  ( -25.37540678000427263, -68.44634676501046044, 7.500000000000000000 ) ) ;
#6555 = EDGE_CURVE ( 'NONE', #4383, #10528, #21100, .T. ) ;
#6556 = VERTEX_POINT ( 'NONE', #2717 ) ;
#6557 = ORIENTED_EDGE ( 'NONE', *, *, #16470, .F. ) ;
#6558 = ORIENTED_EDGE ( 'NONE', *, *, #17962, .T. ) ;
#6559 = FACE_OUTER_BOUND ( 'NONE', #2459, .T. ) ;
#6560 = EDGE_CURVE ( 'NONE', #1592, #20918, #18798, .T. ) ;
#6561 = DIRECTION ( 'NONE',  ( 0.000000000000000000, 0.000000000000000000, 1.000000000000000000 ) ) ;
#6562 = ORIENTED_EDGE ( 'NONE', *, *, #4846, .F. ) ;
#6563 = DIRECTION ( 'NONE',  ( 1.000000000000000000, 0.000000000000000000, 0.000000000000000000 ) ) ;
#6564 = VERTEX_POINT ( 'NONE', #5774 ) ;
#6565 = DIRECTION ( 'NONE',  ( 1.000000000000000000, 0.000000000000000000, 0.000000000000000000 ) ) ;
#6566 = DIRECTION ( 'NONE',  ( -1.000000000000000000, 0.000000000000000000, 0.000000000000000000 ) ) ;
#6567 = CYLINDRICAL_SURFACE ( 'NONE', #16351, 0.5000000000000000000 ) ;
#6568 = DIRECTION ( 'NONE',  ( 0.000000000000000000, -1.000000000000000000, 0.000000000000000000 ) ) ;
#6569 = ORIENTED_EDGE ( 'NONE', *, *, #878, .F. ) ;
#6570 = CYLINDRICAL_SURFACE ( 'NONE', #15232, 4.351418481279133665 ) ;
#6571 = LINE ( 'NONE', #13362, #3911 ) ;
#6572 = EDGE_CURVE ( 'NONE', #4630, #15132, #7316, .T. ) ;
#6573 = ADVANCED_FACE ( 'NONE', ( #21207 ), #2501, .F. ) ;
#6574 = FACE_OUTER_BOUND ( 'NONE', #18878, .T. ) ;
#6575 = DIRECTION ( 'NONE',  ( -3.052134192567367925E-16, -1.000000000000000000, 0.000000000000000000 ) ) ;
#6576 = VERTEX_POINT ( 'NONE', #12656 ) ;
#6577 = CARTESIAN_POINT ( 'NONE',  ( -3.127054932750481964, -32.11873716947361856, 68.00000000000000000 ) ) ;
#6578 = ORIENTED_EDGE ( 'NONE', *, *, #3030, .T. ) ;
#6579 = CARTESIAN_POINT ( 'NONE',  ( -8.638906393579159015, 41.43704565779017202, 70.88527860057354246 ) ) ;
#6580 = DIRECTION ( 'NONE',  ( 1.000000000000000000, 0.000000000000000000, 0.000000000000000000 ) ) ;
#6581 = ORIENTED_EDGE ( 'NONE', *, *, #878, .T. ) ;
#6582 = ORIENTED_EDGE ( 'NONE', *, *, #18700, .T. ) ;
#6583 = VERTEX_POINT ( 'NONE', #16135 ) ;
#6584 = CARTESIAN_POINT ( 'NONE',  ( -1.724728116533986721, 43.31054587065082728, 51.80876104995653719 ) ) ;
#6585 = DIRECTION ( 'NONE',  ( 1.000000000000000000, 0.000000000000000000, 0.000000000000000000 ) ) ;
#6586 = AXIS2_PLACEMENT_3D ( 'NONE', #21530, #17336, #7075 ) ;
#6587 = EDGE_LOOP ( 'NONE', ( #10917, #5815, #6542, #3930 ) ) ;
#6588 = DIRECTION ( 'NONE',  ( 0.000000000000000000, -0.000000000000000000, -1.000000000000000000 ) ) ;
#6589 = ORIENTED_EDGE ( 'NONE', *, *, #5363, .F. ) ;
#6590 = ORIENTED_EDGE ( 'NONE', *, *, #12969, .F. ) ;
#6591 = DIRECTION ( 'NONE',  ( -2.105859220307292343E-16, 1.000000000000000000, -0.000000000000000000 ) ) ;
#6592 = TOROIDAL_SURFACE ( 'NONE', #19079, 2.299999999999993161, 0.2999999999999999889 ) ;
#6593 = CARTESIAN_POINT ( 'NONE',  ( 29.50000000000002132, -2.473451120191013430, -150.0833101980363722 ) ) ;
#6594 = CARTESIAN_POINT ( 'NONE',  ( -27.67540678000428400, -10.94079601157914716, 13.79999999999999893 ) ) ;
#6595 = DIRECTION ( 'NONE',  ( -0.000000000000000000, 1.000000000000000000, -0.000000000000000000 ) ) ;
#6596 = DIRECTION ( 'NONE',  ( -0.000000000000000000, 1.000000000000000000, -0.000000000000000000 ) ) ;
#6597 = CARTESIAN_POINT ( 'NONE',  ( 1.724728116533979838, 42.31054587065082728, 53.66679706732590915 ) ) ;
#6598 = APPLICATION_CONTEXT ( 'automotive_design' ) ;
#6599 = CIRCLE ( 'NONE', #8729, 0.2499999999999977796 ) ;
#6600 = CARTESIAN_POINT ( 'NONE',  ( -21.67365502786443088, 45.72430987248279166, 68.25000000000000000 ) ) ;
#6601 = CARTESIAN_POINT ( 'NONE',  ( -25.37540678000429040, -36.74634676501047181, 42.50000000000000000 ) ) ;
#6602 = AXIS2_PLACEMENT_3D ( 'NONE', #13978, #5170, #18699 ) ;
#6603 = ORIENTED_EDGE ( 'NONE', *, *, #3916, .T. ) ;
#6604 = EDGE_CURVE ( 'NONE', #20393, #14744, #13993, .T. ) ;
#6605 = DIRECTION ( 'NONE',  ( 0.000000000000000000, 0.000000000000000000, -1.000000000000000000 ) ) ;
#6606 = EDGE_LOOP ( 'NONE', ( #18193, #507, #22052, #15089 ) ) ;
#6607 = DIRECTION ( 'NONE',  ( 0.000000000000000000, 0.000000000000000000, 1.000000000000000000 ) ) ;
#6608 = DIRECTION ( 'NONE',  ( 0.000000000000000000, 0.000000000000000000, 1.000000000000000000 ) ) ;
#6609 = VERTEX_POINT ( 'NONE', #16578 ) ;
#6610 = ORIENTED_EDGE ( 'NONE', *, *, #4453, .F. ) ;
#6611 = DIRECTION ( 'NONE',  ( 1.000000000000000000, 0.000000000000000000, 0.000000000000000000 ) ) ;
#6612 = EDGE_CURVE ( 'NONE', #21055, #104, #8672, .T. ) ;
#6613 = DIRECTION ( 'NONE',  ( 0.000000000000000000, 0.000000000000000000, -1.000000000000000000 ) ) ;
#6614 = CARTESIAN_POINT ( 'NONE',  ( -25.37540678000427263, 68.44634676501046044, 7.500000000000000000 ) ) ;
#6615 = CARTESIAN_POINT ( 'NONE',  ( -29.69597781366221412, 25.99124249474150972, 70.50000000000000000 ) ) ;
#6616 = ADVANCED_FACE ( 'NONE', ( #3287 ), #2954, .F. ) ;
#6617 = DIRECTION ( 'NONE',  ( 1.000000000000000000, 0.000000000000000000, 0.000000000000000000 ) ) ;
#6618 = EDGE_CURVE ( 'NONE', #13600, #3729, #22094, .T. ) ;
#6619 = DIRECTION ( 'NONE',  ( -4.336808689941893885E-15, 0.000000000000000000, 1.000000000000000000 ) ) ;
#6620 = DIRECTION ( 'NONE',  ( 1.000000000000000000, -0.000000000000000000, 0.000000000000000000 ) ) ;
#6621 = CARTESIAN_POINT ( 'NONE',  ( -26.61833302554978786, 9.663695060508649348, 13.79999999999999893 ) ) ;
#6622 = DIRECTION ( 'NONE',  ( 0.000000000000000000, -1.000000000000000000, 0.000000000000000000 ) ) ;
#6623 = CARTESIAN_POINT ( 'NONE',  ( -15.06704456860866870, -51.94509779313090547, 13.50000000000000000 ) ) ;
#6624 = DIRECTION ( 'NONE',  ( 0.000000000000000000, 1.000000000000000000, 0.000000000000000000 ) ) ;
#6625 = VECTOR ( 'NONE', #9257, 1000.000000000000000 ) ;
#6626 = TOROIDAL_SURFACE ( 'NONE', #13390, 0.7000000000000000666, 0.2999999999999999889 ) ;
#6627 = ORIENTED_EDGE ( 'NONE', *, *, #4008, .F. ) ;
#6628 = CYLINDRICAL_SURFACE ( 'NONE', #7759, 0.5000000000000004441 ) ;
#6629 = ORIENTED_EDGE ( 'NONE', *, *, #7960, .F. ) ;
#6630 = PRODUCT_DEFINITION_SHAPE ( 'NONE', 'NONE',  #22169 ) ;
#6631 = CARTESIAN_POINT ( 'NONE',  ( 1.724728116533979616, 42.36054587065083155, 37.76679706732590347 ) ) ;
#6632 = ORIENTED_EDGE ( 'NONE', *, *, #533, .F. ) ;
#6633 = DIRECTION ( 'NONE',  ( 1.000000000000000000, 0.000000000000000000, 0.000000000000000000 ) ) ;
#6634 = ADVANCED_FACE ( 'NONE', ( #4747 ), #21648, .T. ) ;
#6635 = VERTEX_POINT ( 'NONE', #4635 ) ;
#6636 = ORIENTED_EDGE ( 'NONE', *, *, #1594, .T. ) ;
#6637 = ORIENTED_EDGE ( 'NONE', *, *, #7214, .F. ) ;
#6638 = TOROIDAL_SURFACE ( 'NONE', #12676, 1.000000000000000000, 0.5000000000000000000 ) ;
#6639 = ORIENTED_EDGE ( 'NONE', *, *, #21873, .T. ) ;
#6640 = ADVANCED_FACE ( 'NONE', ( #14907 ), #3433, .F. ) ;
#6641 = ADVANCED_FACE ( 'NONE', ( #18490 ), #13571, .F. ) ;
#6642 = LINE ( 'NONE', #15348, #10581 ) ;
#6643 = CARTESIAN_POINT ( 'NONE',  ( -29.50000000000002132, -69.00000000000000000, 1.500000000000000000 ) ) ;
#6644 = EDGE_CURVE ( 'NONE', #10751, #15636, #11774, .T. ) ;
#6645 = CYLINDRICAL_SURFACE ( 'NONE', #14952, 1.826718556943725202 ) ;
#6646 = ORIENTED_EDGE ( 'NONE', *, *, #13667, .F. ) ;
#6647 = DIRECTION ( 'NONE',  ( 1.000000000000000000, -0.000000000000000000, 6.123233995736764803E-17 ) ) ;
#6648 = ADVANCED_FACE ( 'NONE', ( #18606 ), #15128, .T. ) ;
#6649 = CARTESIAN_POINT ( 'NONE',  ( -15.95292532278785913, -50.11873716947361856, 68.00000000000000000 ) ) ;
#6650 = DIRECTION ( 'NONE',  ( 0.000000000000000000, 0.000000000000000000, 1.000000000000000000 ) ) ;
#6651 = DIRECTION ( 'NONE',  ( 1.000000000000000000, 0.000000000000000000, 0.000000000000000000 ) ) ;
#6652 = AXIS2_PLACEMENT_3D ( 'NONE', #18224, #2664, #11395 ) ;
#6653 = DIRECTION ( 'NONE',  ( 1.000000000000000000, 0.000000000000000000, 0.000000000000000000 ) ) ;
#6654 = CIRCLE ( 'NONE', #16640, 0.05000000000000143219 ) ;
#6655 = ORIENTED_EDGE ( 'NONE', *, *, #18939, .T. ) ;
#6656 = VECTOR ( 'NONE', #8782, 1000.000000000000000 ) ;
#6657 = AXIS2_PLACEMENT_3D ( 'NONE', #1638, #3440, #17296 ) ;
#6658 = ORIENTED_EDGE ( 'NONE', *, *, #16185, .F. ) ;
#6659 = LINE ( 'NONE', #3394, #7432 ) ;
#6660 = LINE ( 'NONE', #41, #6759 ) ;
#6661 = EDGE_CURVE ( 'NONE', #19805, #13239, #6261, .T. ) ;
#6662 = CARTESIAN_POINT ( 'NONE',  ( 15.13073201445139127, -52.10286008774955491, 13.87500000000000000 ) ) ;
#6663 = ORIENTED_EDGE ( 'NONE', *, *, #14980, .F. ) ;
#6664 = DIRECTION ( 'NONE',  ( 0.000000000000000000, 0.000000000000000000, -1.000000000000000000 ) ) ;
#6665 = CIRCLE ( 'NONE', #2711, 0.1000000000000028644 ) ;
#6666 = FACE_OUTER_BOUND ( 'NONE', #15816, .T. ) ;
#6667 = DIRECTION ( 'NONE',  ( -6.123233995736764803E-17, 0.000000000000000000, 1.000000000000000000 ) ) ;
#6668 = ADVANCED_FACE ( 'NONE', ( #3177 ), #11949, .T. ) ;
#6669 = VECTOR ( 'NONE', #1116, 1000.000000000000000 ) ;
#6670 = DIRECTION ( 'NONE',  ( 0.000000000000000000, 0.000000000000000000, 1.000000000000000000 ) ) ;
#6671 = VECTOR ( 'NONE', #14240, 1000.000000000000000 ) ;
#6672 = ORIENTED_EDGE ( 'NONE', *, *, #2764, .T. ) ;
#6673 = LINE ( 'NONE', #10360, #9173 ) ;
#6674 = EDGE_CURVE ( 'NONE', #21627, #20211, #12299, .T. ) ;
#6675 = CARTESIAN_POINT ( 'NONE',  ( -27.37540678000427619, 10.94079601157914539, 42.50000000000000000 ) ) ;
#6676 = CARTESIAN_POINT ( 'NONE',  ( -25.37540678000426908, 39.04634676501046187, 13.50000000000000000 ) ) ;
#6677 = DIRECTION ( 'NONE',  ( 0.000000000000000000, 0.000000000000000000, 1.000000000000000000 ) ) ;
#6678 = ORIENTED_EDGE ( 'NONE', *, *, #22130, .T. ) ;
#6679 = CARTESIAN_POINT ( 'NONE',  ( 14.66174975910705847, 42.11054587065083155, 13.50000000000000000 ) ) ;
#6680 = ORIENTED_EDGE ( 'NONE', *, *, #1446, .F. ) ;
#6681 = DIRECTION ( 'NONE',  ( 0.000000000000000000, 0.000000000000000000, -1.000000000000000000 ) ) ;
#6682 = DIRECTION ( 'NONE',  ( 0.000000000000000000, -0.000000000000000000, 1.000000000000000000 ) ) ;
#6683 = AXIS2_PLACEMENT_3D ( 'NONE', #4416, #2862, #21449 ) ;
#6684 = ORIENTED_EDGE ( 'NONE', *, *, #8033, .F. ) ;
#6685 = CIRCLE ( 'NONE', #11301, 0.5999999999999999778 ) ;
#6686 = ORIENTED_EDGE ( 'NONE', *, *, #19934, .F. ) ;
#6687 = AXIS2_PLACEMENT_3D ( 'NONE', #14997, #4600, #11413 ) ;
#6688 = ORIENTED_EDGE ( 'NONE', *, *, #5375, .T. ) ;
#6689 = CYLINDRICAL_SURFACE ( 'NONE', #18849, 6.500000000000002665 ) ;
#6690 = DIRECTION ( 'NONE',  ( 1.000000000000000000, 0.000000000000000000, 0.000000000000000000 ) ) ;
#6691 = ORIENTED_EDGE ( 'NONE', *, *, #5367, .T. ) ;
#6692 = CARTESIAN_POINT ( 'NONE',  ( 17.45292532278785913, 0.000000000000000000, 68.00000000000000000 ) ) ;
#6693 = CIRCLE ( 'NONE', #9181, 0.05000000000000143219 ) ;
#6694 = VERTEX_POINT ( 'NONE', #1372 ) ;
#6695 = EDGE_CURVE ( 'NONE', #17212, #6786, #20187, .T. ) ;
#6696 = ORIENTED_EDGE ( 'NONE', *, *, #17486, .F. ) ;
#6697 = LINE ( 'NONE', #3431, #4698 ) ;
#6698 = VERTEX_POINT ( 'NONE', #13339 ) ;
#6699 = CARTESIAN_POINT ( 'NONE',  ( 29.69597781366221767, 26.24124249474150972, 70.25000000000000000 ) ) ;
#6700 = AXIS2_PLACEMENT_3D ( 'NONE', #7547, #10554, #17373 ) ;
#6701 = CARTESIAN_POINT ( 'NONE',  ( -33.20000000000000284, -85.00000000000000000, 1.200000000000000400 ) ) ;
#6702 = AXIS2_PLACEMENT_3D ( 'NONE', #13470, #15575, #255 ) ;
#6703 = TOROIDAL_SURFACE ( 'NONE', #5995, 5.299999999999999822, 0.2999999999999999889 ) ;
#6704 = AXIS2_PLACEMENT_3D ( 'NONE', #5221, #18981, #7231 ) ;
#6705 = PLANE ( 'NONE',  #15354 ) ;
#6706 = DIRECTION ( 'NONE',  ( -4.336808689941893885E-15, 0.000000000000000000, 1.000000000000000000 ) ) ;
#6707 = ORIENTED_EDGE ( 'NONE', *, *, #3244, .F. ) ;
#6708 = DIRECTION ( 'NONE',  ( -0.000000000000000000, -0.000000000000000000, -1.000000000000000000 ) ) ;
#6709 = ADVANCED_FACE ( 'NONE', ( #4844 ), #4966, .T. ) ;
#6710 = DIRECTION ( 'NONE',  ( 0.000000000000000000, 0.000000000000000000, 1.000000000000000000 ) ) ;
#6711 = CIRCLE ( 'NONE', #14177, 0.2999999999999947153 ) ;
#6712 = DIRECTION ( 'NONE',  ( 1.000000000000000000, 0.000000000000000000, 0.000000000000000000 ) ) ;
#6713 = ORIENTED_EDGE ( 'NONE', *, *, #15873, .F. ) ;
#6714 = DIRECTION ( 'NONE',  ( 2.105859220307292343E-16, -1.000000000000000000, 0.000000000000000000 ) ) ;
#6715 = VECTOR ( 'NONE', #13033, 1000.000000000000000 ) ;
#6716 = LINE ( 'NONE', #18776, #14489 ) ;
#6717 = VERTEX_POINT ( 'NONE', #17032 ) ;
#6718 = DIRECTION ( 'NONE',  ( 0.000000000000000000, -1.000000000000000000, 0.000000000000000000 ) ) ;
#6719 = DIRECTION ( 'NONE',  ( 0.000000000000000000, -1.000000000000000000, 0.000000000000000000 ) ) ;
#6720 = ORIENTED_EDGE ( 'NONE', *, *, #6373, .T. ) ;
#6721 = AXIS2_PLACEMENT_3D ( 'NONE', #13044, #16419, #11260 ) ;
#6722 = AXIS2_PLACEMENT_3D ( 'NONE', #1799, #15210, #12078 ) ;
#6723 = ORIENTED_EDGE ( 'NONE', *, *, #3826, .F. ) ;
#6724 = DIRECTION ( 'NONE',  ( -1.000000000000000000, 0.000000000000000000, 0.000000000000000000 ) ) ;
#6725 = ADVANCED_FACE ( 'NONE', ( #3618 ), #6626, .T. ) ;
#6726 = TOROIDAL_SURFACE ( 'NONE', #18131, 2.767785046117003489, 0.2500000000000000000 ) ;
#6727 = ORIENTED_EDGE ( 'NONE', *, *, #22143, .F. ) ;
#6728 = ADVANCED_FACE ( 'NONE', ( #5185 ), #15359, .T. ) ;
#6729 = AXIS2_PLACEMENT_3D ( 'NONE', #4643, #9445, #21769 ) ;
#6730 = CIRCLE ( 'NONE', #13493, 1.162443609680678280 ) ;
#6731 = CARTESIAN_POINT ( 'NONE',  ( -29.13662752439705272, 0.000000000000000000, 0.000000000000000000 ) ) ;
#6732 = VERTEX_POINT ( 'NONE', #134 ) ;
#6733 = DIRECTION ( 'NONE',  ( -1.038507728162729346E-16, -1.000000000000000000, 1.271805165184275985E-32 ) ) ;
#6734 = CARTESIAN_POINT ( 'NONE',  ( -34.40000000000001279, -84.70000000000001705, 79.39999999999999147 ) ) ;
#6735 = FACE_OUTER_BOUND ( 'NONE', #14914, .T. ) ;
#6736 = CARTESIAN_POINT ( 'NONE',  ( -29.37540678000427619, -4.700000000000000178, 3.799999999999999822 ) ) ;
#6737 = CIRCLE ( 'NONE', #15293, 0.05000000000000143219 ) ;
#6738 = DIRECTION ( 'NONE',  ( 0.000000000000000000, 0.000000000000000000, -1.000000000000000000 ) ) ;
#6739 = DIRECTION ( 'NONE',  ( 1.000000000000000000, 0.000000000000000000, 0.000000000000000000 ) ) ;
#6740 = DIRECTION ( 'NONE',  ( 0.000000000000000000, 1.000000000000000000, -0.000000000000000000 ) ) ;
#6741 = VECTOR ( 'NONE', #12067, 1000.000000000000000 ) ;
#6742 = DIRECTION ( 'NONE',  ( 2.107255972849994642E-16, 0.000000000000000000, 1.000000000000000000 ) ) ;
#6744 = EDGE_CURVE ( 'NONE', #9810, #17039, #16929, .T. ) ;
#6743 = DIRECTION ( 'NONE',  ( 0.000000000000000000, 0.000000000000000000, 1.000000000000000000 ) ) ;
#6745 = CIRCLE ( 'NONE', #14219, 0.2999999999999999889 ) ;
#6746 = DIRECTION ( 'NONE',  ( -1.000000000000000000, 0.000000000000000000, -0.000000000000000000 ) ) ;
#6747 = ORIENTED_EDGE ( 'NONE', *, *, #19216, .F. ) ;
#6748 = CARTESIAN_POINT ( 'NONE',  ( 1.824728116533979705, 43.26054587065083012, 33.66679706732590915 ) ) ;
#6749 = EDGE_LOOP ( 'NONE', ( #5194, #11860, #12985, #10717 ) ) ;
#6750 = ORIENTED_EDGE ( 'NONE', *, *, #7184, .F. ) ;
#6751 = DIRECTION ( 'NONE',  ( -1.000000000000000000, 0.000000000000000000, 0.000000000000000000 ) ) ;
#6752 = CARTESIAN_POINT ( 'NONE',  ( 0.000000000000000000, 0.000000000000000000, 0.000000000000000000 ) ) ;
#6753 = EDGE_CURVE ( 'NONE', #19117, #5989, #10175, .T. ) ;
#6754 = VERTEX_POINT ( 'NONE', #7305 ) ;
#6755 = AXIS2_PLACEMENT_3D ( 'NONE', #14346, #19493, #7434 ) ;
#6756 = TOROIDAL_SURFACE ( 'NONE', #12779, 1.300000000000000044, 0.2999999999999999889 ) ;
#6757 = EDGE_LOOP ( 'NONE', ( #19651, #1391, #10195, #11154 ) ) ;
#6758 = TOROIDAL_SURFACE ( 'NONE', #12784, 1.750000000000000000, 0.2500000000000000000 ) ;
#6759 = VECTOR ( 'NONE', #1595, 1000.000000000000000 ) ;
#6760 = VECTOR ( 'NONE', #15869, 1000.000000000000000 ) ;
#6761 = ORIENTED_EDGE ( 'NONE', *, *, #466, .T. ) ;
#6762 = AXIS2_PLACEMENT_3D ( 'NONE', #1317, #21824, #20477 ) ;
#6763 = DIRECTION ( 'NONE',  ( -1.000000000000000000, -0.000000000000000000, -4.336808689942194441E-15 ) ) ;
#6764 = CARTESIAN_POINT ( 'NONE',  ( -25.37540678000427263, 68.74634676501045760, 3.799999999999999822 ) ) ;
#6765 = CARTESIAN_POINT ( 'NONE',  ( -1.724728116533986721, 43.26054587065083012, 27.70876104995653577 ) ) ;
#6766 = ORIENTED_EDGE ( 'NONE', *, *, #20434, .T. ) ;
#6767 = PLANE ( 'NONE',  #16092 ) ;
#6768 = EDGE_CURVE ( 'NONE', #8987, #8743, #11593, .T. ) ;
#6769 = DIRECTION ( 'NONE',  ( 1.000000000000000000, 0.000000000000000000, 0.000000000000000000 ) ) ;
#6770 = DIRECTION ( 'NONE',  ( -1.000000000000000000, 0.000000000000000000, 0.000000000000000000 ) ) ;
#6771 = CIRCLE ( 'NONE', #12797, 0.2999999999999999889 ) ;
#6772 = CARTESIAN_POINT ( 'NONE',  ( -23.04392555272740850, 2.268071869891183034, 13.22877247997976013 ) ) ;
#6773 = CARTESIAN_POINT ( 'NONE',  ( 29.17540678000427690, 6.499884319688664647, 7.500000000000000000 ) ) ;
#6774 = AXIS2_PLACEMENT_3D ( 'NONE', #16502, #1167, #19996 ) ;
#6775 = ORIENTED_EDGE ( 'NONE', *, *, #17405, .T. ) ;
#6776 = ORIENTED_EDGE ( 'NONE', *, *, #6102, .T. ) ;
#6777 = ORIENTED_EDGE ( 'NONE', *, *, #247, .F. ) ;
#6778 = DIRECTION ( 'NONE',  ( 1.000000000000000000, 0.000000000000000000, 6.123233995736764803E-17 ) ) ;
#6779 = EDGE_CURVE ( 'NONE', #15183, #8916, #10881, .T. ) ;
#6780 = CIRCLE ( 'NONE', #7137, 0.2500000000000002220 ) ;
#6781 = PLANE ( 'NONE',  #6408 ) ;
#6782 = EDGE_CURVE ( 'NONE', #341, #4617, #20628, .T. ) ;
#6783 = ORIENTED_EDGE ( 'NONE', *, *, #13703, .F. ) ;
#6784 = EDGE_CURVE ( 'NONE', #15684, #12849, #19156, .T. ) ;
#6785 = CARTESIAN_POINT ( 'NONE',  ( 14.96174975910705918, -51.76873716947361714, 13.79999999999999716 ) ) ;
#6786 = VERTEX_POINT ( 'NONE', #12104 ) ;
#6787 = CARTESIAN_POINT ( 'NONE',  ( 9.141460742840918030, 33.43424481021354921, 7.321391277662001151 ) ) ;
#6788 = CARTESIAN_POINT ( 'NONE',  ( 9.641460742840918030, -32.61873716947361856, 109.6002446535588319 ) ) ;
#6789 = FACE_OUTER_BOUND ( 'NONE', #17388, .T. ) ;
#6790 = CIRCLE ( 'NONE', #18207, 0.2999999999999999334 ) ;
#6791 = CARTESIAN_POINT ( 'NONE',  ( -1.774728116533986544, 43.31054587065082728, 51.80876104995653719 ) ) ;
#6792 = ORIENTED_EDGE ( 'NONE', *, *, #17545, .F. ) ;
#6793 = DIRECTION ( 'NONE',  ( 0.000000000000000000, -1.000000000000000000, 0.000000000000000000 ) ) ;
#6794 = CARTESIAN_POINT ( 'NONE',  ( 9.141460742840918030, -33.43424481021354921, 7.321391277662001151 ) ) ;
#6795 = EDGE_CURVE ( 'NONE', #11408, #17480, #17354, .T. ) ;
#6796 = DIRECTION ( 'NONE',  ( 0.000000000000000000, 0.000000000000000000, 1.000000000000000000 ) ) ;
#6797 = CARTESIAN_POINT ( 'NONE',  ( 1.774728116533979883, 43.26054587065083012, 33.66679706732590915 ) ) ;
#6798 = DIRECTION ( 'NONE',  ( 1.000000000000000000, 0.000000000000000000, 0.000000000000000000 ) ) ;
#6799 = ORIENTED_EDGE ( 'NONE', *, *, #19837, .T. ) ;
#6800 = DIRECTION ( 'NONE',  ( 0.000000000000000000, 0.000000000000000000, -1.000000000000000000 ) ) ;
#6801 = FACE_OUTER_BOUND ( 'NONE', #12373, .T. ) ;
#6802 = ORIENTED_EDGE ( 'NONE', *, *, #14623, .F. ) ;
#6803 = DIRECTION ( 'NONE',  ( 0.000000000000000000, -1.000000000000000000, 0.000000000000000000 ) ) ;
#6804 = CARTESIAN_POINT ( 'NONE',  ( 3.127054932750481964, 32.61873716947361856, 68.00000000000000000 ) ) ;
#6805 = DIRECTION ( 'NONE',  ( 0.000000000000000000, 0.000000000000000000, 1.000000000000000000 ) ) ;
#6806 = ORIENTED_EDGE ( 'NONE', *, *, #7051, .F. ) ;
#6807 = CIRCLE ( 'NONE', #20370, 0.2999999999999999334 ) ;
#6808 = ORIENTED_EDGE ( 'NONE', *, *, #17186, .T. ) ;
#6809 = VERTEX_POINT ( 'NONE', #17251 ) ;
#6810 = FACE_OUTER_BOUND ( 'NONE', #16901, .T. ) ;
#6811 = EDGE_CURVE ( 'NONE', #22008, #19359, #1920, .T. ) ;
#6812 = CARTESIAN_POINT ( 'NONE',  ( -30.37540678000427619, 6.000000000000000000, 3.799999999999999822 ) ) ;
#6813 = AXIS2_PLACEMENT_3D ( 'NONE', #13389, #20348, #16627 ) ;
#6814 = AXIS2_PLACEMENT_3D ( 'NONE', #17079, #14951, #18876 ) ;
#6815 = EDGE_CURVE ( 'NONE', #15052, #3842, #18751, .T. ) ;
#6816 = EDGE_LOOP ( 'NONE', ( #22144, #21213, #11399, #5402 ) ) ;
#6817 = CARTESIAN_POINT ( 'NONE',  ( -1.774728116533986544, 43.31054587065082728, 31.80876104995653719 ) ) ;
#6818 = EDGE_CURVE ( 'NONE', #12110, #7942, #7201, .T. ) ;
#6819 = ORIENTED_EDGE ( 'NONE', *, *, #9878, .F. ) ;
#6820 = CARTESIAN_POINT ( 'NONE',  ( -9.141460742840918030, -32.11873716947361856, 68.00000000000000000 ) ) ;
#6821 = ORIENTED_EDGE ( 'NONE', *, *, #16684, .F. ) ;
#6822 = CARTESIAN_POINT ( 'NONE',  ( -9.178906393579158163, 42.46645089659918426, 67.85468508031152624 ) ) ;
#6823 = DIRECTION ( 'NONE',  ( -6.123233995736764803E-17, 0.000000000000000000, 1.000000000000000000 ) ) ;
#6824 = CARTESIAN_POINT ( 'NONE',  ( -31.50000000000002132, 71.00000000000001421, 1.500000000000000000 ) ) ;
#6825 = PLANE ( 'NONE',  #16146 ) ;
#6826 = ORIENTED_EDGE ( 'NONE', *, *, #14305, .F. ) ;
#6827 = CARTESIAN_POINT ( 'NONE',  ( -9.178906393579158163, 42.46645089659918426, 74.06027860057353962 ) ) ;
#6828 = DIRECTION ( 'NONE',  ( 0.000000000000000000, 1.000000000000000000, -0.000000000000000000 ) ) ;
#6829 = CIRCLE ( 'NONE', #5023, 4.193574995607837863 ) ;
#6830 = EDGE_CURVE ( 'NONE', #4063, #20326, #14806, .T. ) ;
#6831 = CARTESIAN_POINT ( 'NONE',  ( -23.02398829872513986, 2.157133568460765538, 7.500000000000000000 ) ) ;
#6832 = FACE_OUTER_BOUND ( 'NONE', #2700, .T. ) ;
#6833 = EDGE_LOOP ( 'NONE', ( #19841, #11422, #5883, #5486 ) ) ;
#6834 = EDGE_CURVE ( 'NONE', #21631, #3171, #1948, .T. ) ;
#6835 = DIRECTION ( 'NONE',  ( 1.000000000000000000, 0.000000000000000000, -2.388292521039847891E-16 ) ) ;
#6836 = ADVANCED_FACE ( 'NONE', ( #21404 ), #6190, .T. ) ;
#6837 = ORIENTED_EDGE ( 'NONE', *, *, #1809, .F. ) ;
#6838 = DIRECTION ( 'NONE',  ( -0.000000000000000000, -0.000000000000000000, 1.000000000000000000 ) ) ;
#6839 = LINE ( 'NONE', #20579, #21028 ) ;
#6840 = VERTEX_POINT ( 'NONE', #12748 ) ;
#6841 = CARTESIAN_POINT ( 'NONE',  ( -9.718906393579157310, 40.01645089659919563, 70.88527860057354246 ) ) ;
#6842 = ADVANCED_FACE ( 'NONE', ( #12533 ), #14332, .T. ) ;
#6843 = CIRCLE ( 'NONE', #12150, 0.3000000000000016542 ) ;
#6844 = VECTOR ( 'NONE', #5954, 1000.000000000000000 ) ;
#6845 = EDGE_LOOP ( 'NONE', ( #11245, #19925, #10434, #434 ) ) ;
#6846 = CARTESIAN_POINT ( 'NONE',  ( 32.50000000000002132, -71.00000000000001421, 3.200000000000000178 ) ) ;
#6847 = ORIENTED_EDGE ( 'NONE', *, *, #3348, .F. ) ;
#6848 = DIRECTION ( 'NONE',  ( 0.000000000000000000, 0.000000000000000000, -1.000000000000000000 ) ) ;
#6849 = CARTESIAN_POINT ( 'NONE',  ( 15.21174975910705918, 41.81054587065082728, 13.50000000000000000 ) ) ;
#6850 = CARTESIAN_POINT ( 'NONE',  ( -34.39999999999999858, -85.00000000000000000, 0.3000000000000000444 ) ) ;
#6851 = FACE_OUTER_BOUND ( 'NONE', #5344, .T. ) ;
#6852 = DIRECTION ( 'NONE',  ( 0.000000000000000000, 0.000000000000000000, -1.000000000000000000 ) ) ;
#6853 = CARTESIAN_POINT ( 'NONE',  ( 8.641460742840918030, 32.93424481021354921, 7.321391277662001151 ) ) ;
#6854 = ADVANCED_FACE ( 'NONE', ( #19712 ), #6077, .T. ) ;
#6855 = CIRCLE ( 'NONE', #20768, 1.299999999999999156 ) ;
#6856 = DIRECTION ( 'NONE',  ( 0.000000000000000000, -1.000000000000000000, 0.000000000000000000 ) ) ;
#6857 = ADVANCED_FACE ( 'NONE', ( #795 ), #10770, .F. ) ;
#6858 = CARTESIAN_POINT ( 'NONE',  ( -15.21174975910705029, -52.10286008774955491, 13.87500000000000000 ) ) ;
#6859 = ADVANCED_FACE ( 'NONE', ( #16111 ), #4382, .F. ) ;
#6860 = ORIENTED_EDGE ( 'NONE', *, *, #18942, .T. ) ;
#6861 = FACE_OUTER_BOUND ( 'NONE', #2614, .T. ) ;
#6862 = FACE_OUTER_BOUND ( 'NONE', #16090, .T. ) ;
#6863 = CARTESIAN_POINT ( 'NONE',  ( 34.69999999999999574, 85.00000000000000000, 0.6000000000000037526 ) ) ;
#6864 = ORIENTED_EDGE ( 'NONE', *, *, #17654, .F. ) ;
#6865 = VERTEX_POINT ( 'NONE', #14545 ) ;
#6866 = DIRECTION ( 'NONE',  ( 1.000000000000000000, 0.000000000000000000, 0.000000000000000000 ) ) ;
#6867 = AXIS2_PLACEMENT_3D ( 'NONE', #9701, #18065, #11361 ) ;
#6868 = ORIENTED_EDGE ( 'NONE', *, *, #2706, .T. ) ;
#6869 = AXIS2_PLACEMENT_3D ( 'NONE', #8787, #17385, #12331 ) ;
#6870 = EDGE_LOOP ( 'NONE', ( #9845, #21861, #10315, #10962 ) ) ;
#6871 = EDGE_CURVE ( 'NONE', #5089, #2540, #8399, .T. ) ;
#6872 = ORIENTED_EDGE ( 'NONE', *, *, #19919, .T. ) ;
#6873 = DIRECTION ( 'NONE',  ( 0.000000000000000000, -1.000000000000000000, 0.000000000000000000 ) ) ;
#6874 = DIRECTION ( 'NONE',  ( 0.000000000000000000, 0.000000000000000000, -1.000000000000000000 ) ) ;
#6875 = DIRECTION ( 'NONE',  ( 0.000000000000000000, -1.000000000000000000, 0.000000000000000000 ) ) ;
#6876 = FACE_OUTER_BOUND ( 'NONE', #2957, .T. ) ;
#6877 = DIRECTION ( 'NONE',  ( 0.000000000000000000, -0.000000000000000000, 1.000000000000000000 ) ) ;
#6878 = EDGE_CURVE ( 'NONE', #5446, #5867, #10871, .T. ) ;
#6879 = AXIS2_PLACEMENT_3D ( 'NONE', #12777, #14574, #2609 ) ;
#6880 = CARTESIAN_POINT ( 'NONE',  ( -31.44597781366222122, 56.94165929845684815, 70.25000000000000000 ) ) ;
#6881 = AXIS2_PLACEMENT_3D ( 'NONE', #7059, #5268, #17122 ) ;
#6882 = FACE_OUTER_BOUND ( 'NONE', #12193, .T. ) ;
#6884 = EDGE_CURVE ( 'NONE', #15579, #13135, #2690, .T. ) ;
#6883 =( BOUNDED_CURVE ( )  B_SPLINE_CURVE ( 3, ( #16488, #21216, #14364, #14588 ),
 .UNSPECIFIED., .F., .T. ) 
 B_SPLINE_CURVE_WITH_KNOTS ( ( 4, 4 ),
 ( 4.712388980384689674, 6.283185307179586232 ),
 .UNSPECIFIED. ) 
 CURVE ( )  GEOMETRIC_REPRESENTATION_ITEM ( )  RATIONAL_B_SPLINE_CURVE ( ( 1.000000000000000000, 0.8047378541243649375, 0.8047378541243649375, 1.000000000000000000 ) ) 
 REPRESENTATION_ITEM ( '' )  );
#6885 = DIRECTION ( 'NONE',  ( 0.000000000000000000, 0.000000000000000000, -1.000000000000000000 ) ) ;
#6886 = FACE_OUTER_BOUND ( 'NONE', #20772, .T. ) ;
#6887 = ORIENTED_EDGE ( 'NONE', *, *, #12213, .F. ) ;
#6888 = CARTESIAN_POINT ( 'NONE',  ( -1.724728116533986721, 42.36054587065083155, 29.71679706732590631 ) ) ;
#6889 = EDGE_LOOP ( 'NONE', ( #7898, #6428, #1290, #390 ) ) ;
#6890 = ORIENTED_EDGE ( 'NONE', *, *, #5831, .T. ) ;
#6891 = ORIENTED_EDGE ( 'NONE', *, *, #8803, .F. ) ;
#6892 = CARTESIAN_POINT ( 'NONE',  ( -7.347880794884131322E-17, -84.70000000000001705, 1.200000000000002176 ) ) ;
#6893 = SHAPE_REPRESENTATION_RELATIONSHIP ( 'NONE' , 'NONE' ,  #3995, #2184 ) ;
#6894 = DIRECTION ( 'NONE',  ( -0.000000000000000000, 0.000000000000000000, 1.000000000000000000 ) ) ;
#6895 = ORIENTED_EDGE ( 'NONE', *, *, #8561, .F. ) ;
#6896 = LINE ( 'NONE', #18384, #4142 ) ;
#6897 = APPLICATION_CONTEXT ( 'automotive_design' ) ;
#6898 = CIRCLE ( 'NONE', #12924, 0.5000000000000004441 ) ;
#6899 = VECTOR ( 'NONE', #5129, 1000.000000000000000 ) ;
#6900 = DIRECTION ( 'NONE',  ( 0.000000000000000000, 1.000000000000000000, 0.000000000000000000 ) ) ;
#6901 = DIRECTION ( 'NONE',  ( -1.000000000000000000, 0.000000000000000000, 0.000000000000000000 ) ) ;
#6902 = DIRECTION ( 'NONE',  ( -6.123233995736764803E-17, 0.000000000000000000, 1.000000000000000000 ) ) ;
#6903 = ORIENTED_EDGE ( 'NONE', *, *, #3235, .T. ) ;
#6904 = FACE_OUTER_BOUND ( 'NONE', #4345, .T. ) ;
#6905 = CARTESIAN_POINT ( 'NONE',  ( 29.50000000000002132, 69.00000000000000000, 0.2999999999999947153 ) ) ;
#6906 = ADVANCED_FACE ( 'NONE', ( #9416 ), #4818, .T. ) ;
#6907 = DIRECTION ( 'NONE',  ( 1.000000000000000000, 0.000000000000000000, 0.000000000000000000 ) ) ;
#6908 = DIRECTION ( 'NONE',  ( -1.000000000000000000, 0.000000000000000000, -6.123233995736764803E-17 ) ) ;
#6909 = CARTESIAN_POINT ( 'NONE',  ( 1.774728116533979660, 42.31054587065082728, 49.66679706732590915 ) ) ;
#6910 = ORIENTED_EDGE ( 'NONE', *, *, #4734, .T. ) ;
#6911 = CYLINDRICAL_SURFACE ( 'NONE', #17342, 0.2999999999999999334 ) ;
#6912 = DIRECTION ( 'NONE',  ( 0.000000000000000000, 0.000000000000000000, 1.000000000000000000 ) ) ;
#6913 = ORIENTED_EDGE ( 'NONE', *, *, #5717, .F. ) ;
#6914 = CYLINDRICAL_SURFACE ( 'NONE', #11104, 0.3000000000000016542 ) ;
#6915 = CYLINDRICAL_SURFACE ( 'NONE', #887, 0.5000000000000004441 ) ;
#6916 = CARTESIAN_POINT ( 'NONE',  ( 29.20000000000002061, -68.70000000000001705, 0.000000000000000000 ) ) ;
#6917 = ORIENTED_EDGE ( 'NONE', *, *, #6974, .T. ) ;
#6918 = ORIENTED_EDGE ( 'NONE', *, *, #401, .T. ) ;
#6919 = EDGE_LOOP ( 'NONE', ( #2983, #13168, #14194, #18537 ) ) ;
#6920 = DIRECTION ( 'NONE',  ( 0.000000000000000000, 1.000000000000000000, 0.000000000000000000 ) ) ;
#6921 = CARTESIAN_POINT ( 'NONE',  ( -8.638906393579159015, 43.51045099701597252, 68.06527860057354928 ) ) ;
#6922 = LINE ( 'NONE', #1406, #20025 ) ;
#6923 = DIRECTION ( 'NONE',  ( 0.000000000000000000, 0.000000000000000000, 1.000000000000000000 ) ) ;
#6924 = EDGE_CURVE ( 'NONE', #13253, #15404, #162, .T. ) ;
#6925 = VERTEX_POINT ( 'NONE', #7637 ) ;
#6926 = LINE ( 'NONE', #15500, #7915 ) ;
#6927 = ORIENTED_EDGE ( 'NONE', *, *, #1494, .F. ) ;
#6928 = CARTESIAN_POINT ( 'NONE',  ( -30.07540678000427548, 6.000000000000000000, 7.500000000000000000 ) ) ;
#6929 = CARTESIAN_POINT ( 'NONE',  ( 30.79999999999999716, -84.70000000000001705, 0.3000000000000039857 ) ) ;
#6930 = DIRECTION ( 'NONE',  ( 0.000000000000000000, 0.000000000000000000, 1.000000000000000000 ) ) ;
#6931 = FACE_OUTER_BOUND ( 'NONE', #8900, .T. ) ;
#6932 = ORIENTED_EDGE ( 'NONE', *, *, #15370, .F. ) ;
#6933 = CARTESIAN_POINT ( 'NONE',  ( 15.95292532278785913, 52.11873716947361856, 68.00000000000000000 ) ) ;
#6934 = DIRECTION ( 'NONE',  ( 1.000000000000000000, 0.000000000000000000, 0.000000000000000000 ) ) ;
#6935 = EDGE_CURVE ( 'NONE', #1047, #2833, #7685, .T. ) ;
#6936 = EDGE_CURVE ( 'NONE', #21686, #4773, #21519, .T. ) ;
#6937 = ADVANCED_FACE ( 'NONE', ( #17588 ), #3031, .T. ) ;
#6938 = CARTESIAN_POINT ( 'NONE',  ( -1.824728116533986810, 42.36054587065083155, 41.76679706732590347 ) ) ;
#6939 = CARTESIAN_POINT ( 'NONE',  ( 1.824728116533979261, 42.36054587065083155, 27.80876104995653719 ) ) ;
#6940 = ORIENTED_EDGE ( 'NONE', *, *, #13166, .F. ) ;
#6941 = LINE ( 'NONE', #3116, #15882 ) ;
#6942 = EDGE_CURVE ( 'NONE', #311, #14884, #9086, .T. ) ;
#6943 = CARTESIAN_POINT ( 'NONE',  ( 33.49999999999998579, 85.00000000000000000, 78.20000000000000284 ) ) ;
#6944 = ORIENTED_EDGE ( 'NONE', *, *, #20037, .F. ) ;
#6945 = CARTESIAN_POINT ( 'NONE',  ( 0.000000000000000000, -39.04634676501046187, 13.50000000000000000 ) ) ;
#6946 = ORIENTED_EDGE ( 'NONE', *, *, #6041, .T. ) ;
#6947 = CARTESIAN_POINT ( 'NONE',  ( -33.50000000000001421, 85.00000000000000000, 78.79999999999999716 ) ) ;
#6948 = EDGE_CURVE ( 'NONE', #13437, #471, #16969, .T. ) ;
#6949 = ORIENTED_EDGE ( 'NONE', *, *, #12466, .T. ) ;
#6950 = DIRECTION ( 'NONE',  ( 1.224646799147353207E-16, 0.000000000000000000, 1.000000000000000000 ) ) ;
#6951 = ORIENTED_EDGE ( 'NONE', *, *, #21583, .T. ) ;
#6952 = CARTESIAN_POINT ( 'NONE',  ( -9.718906393579157310, 43.51045099701597252, 68.06527860057354928 ) ) ;
#6953 =( GEOMETRIC_REPRESENTATION_CONTEXT ( 3 ) GLOBAL_UNCERTAINTY_ASSIGNED_CONTEXT ( ( #10515 ) ) GLOBAL_UNIT_ASSIGNED_CONTEXT ( ( #8855, #19140, #15452 ) ) REPRESENTATION_CONTEXT ( 'NONE', 'WORKASPACE' ) );
#6954 = LINE ( 'NONE', #3690, #2932 ) ;
#6955 = CARTESIAN_POINT ( 'NONE',  ( 1.774728116533979438, 42.31054587065082728, 47.80876104995653719 ) ) ;
#6956 = EDGE_CURVE ( 'NONE', #18789, #8135, #9648, .T. ) ;
#6957 = FACE_OUTER_BOUND ( 'NONE', #11930, .T. ) ;
#6958 = EDGE_CURVE ( 'NONE', #6698, #12463, #19822, .T. ) ;
#6959 = CIRCLE ( 'NONE', #9800, 0.05000000000000143219 ) ;
#6960 = CARTESIAN_POINT ( 'NONE',  ( 3.627054932750481964, -33.43424481021354921, 7.321391277662001151 ) ) ;
#6961 = CARTESIAN_POINT ( 'NONE',  ( -28.57540678000427548, -6.776800961815481195, 13.50000000000000000 ) ) ;
#6962 = ORIENTED_EDGE ( 'NONE', *, *, #3922, .T. ) ;
#6963 = CARTESIAN_POINT ( 'NONE',  ( 29.17540678000427690, -6.499884319688664647, 7.500000000000000000 ) ) ;
#6964 = CYLINDRICAL_SURFACE ( 'NONE', #5979, 0.1000000000000028644 ) ;
#6965 = CARTESIAN_POINT ( 'NONE',  ( -1.824728116533986810, 42.36054587065083155, 39.70876104995653577 ) ) ;
#6966 = CARTESIAN_POINT ( 'NONE',  ( -9.641460742840918030, -32.61873716947361856, 68.00000000000000000 ) ) ;
#6967 = ORIENTED_EDGE ( 'NONE', *, *, #14773, .F. ) ;
#6968 = ORIENTED_EDGE ( 'NONE', *, *, #14902, .F. ) ;
#6969 = DIRECTION ( 'NONE',  ( 0.000000000000000000, 0.000000000000000000, 1.000000000000000000 ) ) ;
#6970 = CARTESIAN_POINT ( 'NONE',  ( 27.13561920550106521, 5.281294294914841814, 81.99999999999998579 ) ) ;
#6971 = VERTEX_POINT ( 'NONE', #4485 ) ;
#6972 =( NAMED_UNIT ( * ) SI_UNIT ( $, .STERADIAN. ) SOLID_ANGLE_UNIT ( ) );
#6973 = ORIENTED_EDGE ( 'NONE', *, *, #775, .F. ) ;
#6974 = EDGE_CURVE ( 'NONE', #17660, #4505, #13318, .T. ) ;
#6975 = ORIENTED_EDGE ( 'NONE', *, *, #8325, .T. ) ;
#6976 = EDGE_CURVE ( 'NONE', #15626, #961, #12662, .T. ) ;
#6977 = ORIENTED_EDGE ( 'NONE', *, *, #10120, .F. ) ;
#6978 = DIRECTION ( 'NONE',  ( 0.000000000000000000, 0.000000000000000000, 1.000000000000000000 ) ) ;
#6979 = FACE_OUTER_BOUND ( 'NONE', #18869, .T. ) ;
#6980 = LINE ( 'NONE', #28, #20695 ) ;
#6981 = AXIS2_PLACEMENT_3D ( 'NONE', #4053, #18016, #11089 ) ;
#6982 = EDGE_CURVE ( 'NONE', #19753, #11635, #4659, .T. ) ;
#6983 = DIRECTION ( 'NONE',  ( 1.000000000000000000, 0.000000000000000000, -0.000000000000000000 ) ) ;
#6984 = DIRECTION ( 'NONE',  ( 0.000000000000000000, 0.000000000000000000, 1.000000000000000000 ) ) ;
#6985 = DIRECTION ( 'NONE',  ( -0.000000000000000000, -1.000000000000000000, -0.000000000000000000 ) ) ;
#6986 = CARTESIAN_POINT ( 'NONE',  ( 9.141460742840918030, 32.93424481021354921, 42.50000000000000000 ) ) ;
#6987 = CARTESIAN_POINT ( 'NONE',  ( -1.724728116533986721, 42.31054587065082728, 53.71679706732590631 ) ) ;
#6988 = ORIENTED_EDGE ( 'NONE', *, *, #20469, .F. ) ;
#6989 = ORIENTED_EDGE ( 'NONE', *, *, #17372, .F. ) ;
#6990 = CARTESIAN_POINT ( 'NONE',  ( 9.141460742840918030, 33.43424481021354921, 42.50000000000000000 ) ) ;
#6991 = ORIENTED_EDGE ( 'NONE', *, *, #13157, .T. ) ;
#6992 = AXIS2_PLACEMENT_3D ( 'NONE', #13155, #4332, #11144 ) ;
#6993 = VECTOR ( 'NONE', #18433, 1000.000000000000000 ) ;
#6994 = EDGE_CURVE ( 'NONE', #13036, #11265, #3045, .T. ) ;
#6995 = CARTESIAN_POINT ( 'NONE',  ( -9.178906393579158163, 42.46645089659918426, 67.75164986378473486 ) ) ;
#6996 = EDGE_CURVE ( 'NONE', #299, #10408, #16785, .T. ) ;
#6997 = CARTESIAN_POINT ( 'NONE',  ( 28.87540678000427619, -63.74634676501045050, 13.50000000000000000 ) ) ;
#6998 = CARTESIAN_POINT ( 'NONE',  ( -1.774728116533986766, 42.36054587065083155, 39.80876104995653719 ) ) ;
#6999 = FACE_OUTER_BOUND ( 'NONE', #1717, .T. ) ;
#7000 = VECTOR ( 'NONE', #18775, 1000.000000000000000 ) ;
#7001 = VERTEX_POINT ( 'NONE', #4937 ) ;
#7002 = DIRECTION ( 'NONE',  ( 0.000000000000000000, 0.000000000000000000, 1.000000000000000000 ) ) ;
#7003 = FACE_OUTER_BOUND ( 'NONE', #4021, .T. ) ;
#7004 = CARTESIAN_POINT ( 'NONE',  ( -14.96174975910705207, 51.86873716947361856, 14.00000000000000000 ) ) ;
#7005 = DIRECTION ( 'NONE',  ( -0.000000000000000000, -0.000000000000000000, 1.000000000000000000 ) ) ;
#7006 = CARTESIAN_POINT ( 'NONE',  ( -27.67540678000426979, 36.74634676501047181, 13.50000000000000000 ) ) ;
#7007 = DIRECTION ( 'NONE',  ( 0.000000000000000000, 0.000000000000000000, 1.000000000000000000 ) ) ;
#7008 = CIRCLE ( 'NONE', #13405, 0.2999999999999999334 ) ;
#7009 = AXIS2_PLACEMENT_3D ( 'NONE', #15936, #19423, #12354 ) ;
#7010 = CARTESIAN_POINT ( 'NONE',  ( -18.91037735075775217, 42.46645089659918426, 68.25000000000000000 ) ) ;
#7011 = CARTESIAN_POINT ( 'NONE',  ( -26.37540678000427619, 10.94079601157914539, 42.50000000000000000 ) ) ;
#7012 = DIRECTION ( 'NONE',  ( 1.000000000000000000, 0.000000000000000000, 0.000000000000000000 ) ) ;
#7013 = EDGE_CURVE ( 'NONE', #17752, #4113, #18028, .T. ) ;
#7014 = ORIENTED_EDGE ( 'NONE', *, *, #19930, .F. ) ;
#7015 = ORIENTED_EDGE ( 'NONE', *, *, #8966, .T. ) ;
#7016 = ORIENTED_EDGE ( 'NONE', *, *, #7247, .F. ) ;
#7017 = DIRECTION ( 'NONE',  ( 1.000000000000000000, 0.000000000000000000, 0.000000000000000000 ) ) ;
#7018 = CARTESIAN_POINT ( 'NONE',  ( -25.37540678000427263, 63.74634676501045050, 7.799999999999999822 ) ) ;
#7019 = DIRECTION ( 'NONE',  ( 0.000000000000000000, 1.000000000000000000, 0.000000000000000000 ) ) ;
#7020 = CARTESIAN_POINT ( 'NONE',  ( -4.603906393579157097, 42.46645089659918426, 70.88527860057354246 ) ) ;
#7021 = AXIS2_PLACEMENT_3D ( 'NONE', #8973, #19270, #10762 ) ;
#7022 = EDGE_CURVE ( 'NONE', #16813, #6358, #19834, .T. ) ;
#7023 = EDGE_CURVE ( 'NONE', #19849, #9049, #871, .T. ) ;
#7024 = EDGE_LOOP ( 'NONE', ( #11777, #337, #20519, #293 ) ) ;
#7025 = DIRECTION ( 'NONE',  ( -2.832483164223434527E-16, -1.000000000000000000, 0.000000000000000000 ) ) ;
#7026 = VECTOR ( 'NONE', #16372, 1000.000000000000000 ) ;
#7027 = EDGE_LOOP ( 'NONE', ( #17868, #13662, #21501, #17323 ) ) ;
#7028 = CARTESIAN_POINT ( 'NONE',  ( 15.95292532278785913, 51.61873716947361856, 68.00000000000000000 ) ) ;
#7029 = CARTESIAN_POINT ( 'NONE',  ( -32.23382792203229741, 83.71979900898287497, 68.25000000000000000 ) ) ;
#7030 = CARTESIAN_POINT ( 'NONE',  ( -29.69597781366221767, 56.94165929845684815, 70.25000000000000000 ) ) ;
#7031 = DIRECTION ( 'NONE',  ( 2.107255972849994642E-16, -0.000000000000000000, 1.000000000000000000 ) ) ;
#7032 = ORIENTED_EDGE ( 'NONE', *, *, #10120, .T. ) ;
#7033 = CARTESIAN_POINT ( 'NONE',  ( 23.06502549581203709, 2.381505846144868155, 13.31536975879941131 ) ) ;
#7034 = DIRECTION ( 'NONE',  ( 1.000000000000000000, 0.000000000000000000, 0.000000000000000000 ) ) ;
#7035 = DIRECTION ( 'NONE',  ( 1.000000000000000000, 0.000000000000000000, 0.000000000000000000 ) ) ;
#7036 = CARTESIAN_POINT ( 'NONE',  ( 34.69999999999999574, 84.70000000000001705, 0.6000000000000037526 ) ) ;
#7037 = ORIENTED_EDGE ( 'NONE', *, *, #20493, .T. ) ;
#7038 = AXIS2_PLACEMENT_3D ( 'NONE', #2587, #4477, #9411 ) ;
#7039 = VECTOR ( 'NONE', #5811, 1000.000000000000000 ) ;
#7040 = DIRECTION ( 'NONE',  ( -1.000000000000000000, 0.000000000000000000, 0.000000000000000000 ) ) ;
#7041 = AXIS2_PLACEMENT_3D ( 'NONE', #4448, #11492, #14741 ) ;
#7042 = EDGE_CURVE ( 'NONE', #9421, #10522, #9462, .T. ) ;
#7043 = CARTESIAN_POINT ( 'NONE',  ( -1.724728116533986721, 43.26054587065083012, 41.76679706732590347 ) ) ;
#7044 = VERTEX_POINT ( 'NONE', #9975 ) ;
#7045 = AXIS2_PLACEMENT_3D ( 'NONE', #9759, #21408, #6193 ) ;
#7046 = CARTESIAN_POINT ( 'NONE',  ( -11.94625475753432120, -2.835528047479821900, 13.74999999999999822 ) ) ;
#7047 = DIRECTION ( 'NONE',  ( 1.000000000000000000, 0.000000000000000000, 0.000000000000000000 ) ) ;
#7048 = ORIENTED_EDGE ( 'NONE', *, *, #4103, .F. ) ;
#7049 = EDGE_CURVE ( 'NONE', #13197, #6444, #12298, .T. ) ;
#7050 = EDGE_CURVE ( 'NONE', #22112, #18107, #12058, .T. ) ;
#7051 = EDGE_CURVE ( 'NONE', #11610, #8448, #18400, .T. ) ;
#7052 = ORIENTED_EDGE ( 'NONE', *, *, #10613, .T. ) ;
#7053 = AXIS2_PLACEMENT_3D ( 'NONE', #6342, #21785, #1166 ) ;
#7054 = CIRCLE ( 'NONE', #12381, 0.05000000000000143219 ) ;
#7055 = AXIS2_PLACEMENT_3D ( 'NONE', #6381, #761, #21254 ) ;
#7056 = ORIENTED_EDGE ( 'NONE', *, *, #21778, .F. ) ;
#7057 = CARTESIAN_POINT ( 'NONE',  ( 31.44597781366222122, 56.94165929845684104, 70.25000000000000000 ) ) ;
#7058 = AXIS2_PLACEMENT_3D ( 'NONE', #1950, #10374, #13492 ) ;
#7059 = CARTESIAN_POINT ( 'NONE',  ( 29.17540678000427690, 0.000000000000000000, 7.799999999999999822 ) ) ;
#7060 = FACE_OUTER_BOUND ( 'NONE', #15858, .T. ) ;
#7061 = DIRECTION ( 'NONE',  ( 0.000000000000000000, 0.000000000000000000, -1.000000000000000000 ) ) ;
#7062 = CARTESIAN_POINT ( 'NONE',  ( 29.37540678000427619, -6.000000000000000000, 7.200000000000000178 ) ) ;
#7063 = EDGE_CURVE ( 'NONE', #15586, #19777, #3398, .T. ) ;
#7064 = DIRECTION ( 'NONE',  ( 0.7193398003386525241, -8.809371839840268653E-17, 0.6946583704589959218 ) ) ;
#7065 = DIRECTION ( 'NONE',  ( -0.000000000000000000, 1.000000000000000000, -0.000000000000000000 ) ) ;
#7066 = AXIS2_PLACEMENT_3D ( 'NONE', #999, #11739, #13307 ) ;
#7067 = EDGE_LOOP ( 'NONE', ( #10641, #5295, #5371, #770, #19042, #6324, #3272, #19032 ) ) ;
#7068 = LINE ( 'NONE', #22067, #15974 ) ;
#7069 = FACE_OUTER_BOUND ( 'NONE', #20703, .T. ) ;
#7070 = AXIS2_PLACEMENT_3D ( 'NONE', #17918, #2829, #5970 ) ;
#7071 = ORIENTED_EDGE ( 'NONE', *, *, #11791, .T. ) ;
#7072 = TOROIDAL_SURFACE ( 'NONE', #6729, 0.5999999999999999778, 0.2999999999999999889 ) ;
#7073 = ORIENTED_EDGE ( 'NONE', *, *, #19525, .T. ) ;
#7074 = FACE_OUTER_BOUND ( 'NONE', #3917, .T. ) ;
#7075 = DIRECTION ( 'NONE',  ( 1.000000000000000000, 0.000000000000000000, 0.000000000000000000 ) ) ;
#7076 = ADVANCED_FACE ( 'NONE', ( #18133 ), #4611, .F. ) ;
#7077 = ORIENTED_EDGE ( 'NONE', *, *, #6424, .F. ) ;
#7078 = EDGE_CURVE ( 'NONE', #13976, #13366, #15881, .T. ) ;
#7079 = ADVANCED_FACE ( 'NONE', ( #4816 ), #15103, .T. ) ;
#7080 = CARTESIAN_POINT ( 'NONE',  ( 23.26560317237337117, -3.297643262788042762, 13.49417356369015586 ) ) ;
#7081 = ORIENTED_EDGE ( 'NONE', *, *, #8624, .F. ) ;
#7082 = AXIS2_PLACEMENT_3D ( 'NONE', #7166, #1788, #8627 ) ;
#7083 = VECTOR ( 'NONE', #14063, 1000.000000000000000 ) ;
#7084 = ORIENTED_EDGE ( 'NONE', *, *, #8282, .F. ) ;
#7085 = CARTESIAN_POINT ( 'NONE',  ( 18.22752199202934520, 0.000000000000000000, 13.79999999999999893 ) ) ;
#7086 = FACE_OUTER_BOUND ( 'NONE', #12895, .T. ) ;
#7087 = DIRECTION ( 'NONE',  ( -1.000000000000000000, -3.491481338843133355E-15, 1.224646799147353207E-16 ) ) ;
#7088 = CIRCLE ( 'NONE', #15996, 0.2999999999999999334 ) ;
#7089 = CARTESIAN_POINT ( 'NONE',  ( 23.02398829872513986, 3.262363296411947111, 13.79999999999999716 ) ) ;
#7090 = DIRECTION ( 'NONE',  ( 0.000000000000000000, -0.000000000000000000, 1.000000000000000000 ) ) ;
#7091 = AXIS2_PLACEMENT_3D ( 'NONE', #21292, #19609, #1233 ) ;
#7092 = CARTESIAN_POINT ( 'NONE',  ( 1.724728116533979838, 43.26054587065083012, 49.71679706732589921 ) ) ;
#7093 = EDGE_CURVE ( 'NONE', #1947, #10037, #11961, .T. ) ;
#7094 = DIRECTION ( 'NONE',  ( 0.000000000000000000, 0.000000000000000000, -1.000000000000000000 ) ) ;
#7095 = CARTESIAN_POINT ( 'NONE',  ( 30.49999999999999645, 69.70000000000000284, 0.3000000000000033751 ) ) ;
#7096 = DIRECTION ( 'NONE',  ( -0.000000000000000000, -1.000000000000000000, -0.000000000000000000 ) ) ;
#7097 = CARTESIAN_POINT ( 'NONE',  ( 14.66174975910705847, -51.76873716947361714, 13.50000000000000000 ) ) ;
#7098 = ADVANCED_FACE ( 'NONE', ( #3362 ), #12257, .T. ) ;
#7099 = CARTESIAN_POINT ( 'NONE',  ( -26.37540678000427619, -10.94079601157914716, 13.79999999999999893 ) ) ;
#7100 = CIRCLE ( 'NONE', #12778, 0.5000000000000004441 ) ;
#7101 = AXIS2_PLACEMENT_3D ( 'NONE', #22043, #3122, #5034 ) ;
#7102 = ORIENTED_EDGE ( 'NONE', *, *, #1936, .T. ) ;
#7103 = ORIENTED_EDGE ( 'NONE', *, *, #14455, .F. ) ;
#7104 = CARTESIAN_POINT ( 'NONE',  ( -1.724728116533986721, 43.31054587065082728, 27.75876104995654003 ) ) ;
#7105 = LINE ( 'NONE', #19166, #5283 ) ;
#7106 = ORIENTED_EDGE ( 'NONE', *, *, #18676, .F. ) ;
#7107 = CIRCLE ( 'NONE', #1736, 0.05000000000000143219 ) ;
#7108 = CIRCLE ( 'NONE', #19978, 2.000000000000001776 ) ;
#7109 = AXIS2_PLACEMENT_3D ( 'NONE', #12352, #724, #7351 ) ;
#7110 = EDGE_CURVE ( 'NONE', #9769, #11165, #17315, .T. ) ;
#7111 = CARTESIAN_POINT ( 'NONE',  ( -15.21174975910705207, 52.10286008774954780, 13.87500000000000000 ) ) ;
#7112 = AXIS2_PLACEMENT_3D ( 'NONE', #6033, #12818, #17975 ) ;
#7113 = DIRECTION ( 'NONE',  ( -1.000000000000000000, -0.000000000000000000, -0.000000000000000000 ) ) ;
#7114 = EDGE_LOOP ( 'NONE', ( #21491, #21111, #1499, #17628 ) ) ;
#7115 = DIRECTION ( 'NONE',  ( 0.000000000000000000, 0.000000000000000000, 1.000000000000000000 ) ) ;
#7116 = DIRECTION ( 'NONE',  ( -1.000000000000000000, -0.000000000000000000, -0.000000000000000000 ) ) ;
#7117 = DIRECTION ( 'NONE',  ( 0.000000000000000000, 0.000000000000000000, -1.000000000000000000 ) ) ;
#7118 = VECTOR ( 'NONE', #6828, 1000.000000000000000 ) ;
#7119 = CARTESIAN_POINT ( 'NONE',  ( 1.724728116533979838, 43.26054587065083012, 41.66679706732590915 ) ) ;
#7120 = FACE_OUTER_BOUND ( 'NONE', #20429, .T. ) ;
#7121 = LINE ( 'NONE', #8898, #5216 ) ;
#7122 = AXIS2_PLACEMENT_3D ( 'NONE', #14638, #868, #6388 ) ;
#7123 = EDGE_CURVE ( 'NONE', #1401, #3263, #19433, .T. ) ;
#7124 = CARTESIAN_POINT ( 'NONE',  ( 1.724728116533979616, 43.31054587065082728, 51.80876104995653719 ) ) ;
#7125 = CARTESIAN_POINT ( 'NONE',  ( 29.13662752439705272, 0.000000000000000000, -18.50000000000000000 ) ) ;
#7126 = DIRECTION ( 'NONE',  ( 0.000000000000000000, 1.000000000000000000, 0.000000000000000000 ) ) ;
#7127 = EDGE_CURVE ( 'NONE', #17668, #14491, #19109, .T. ) ;
#7128 = EDGE_LOOP ( 'NONE', ( #16768, #8711, #12536, #9434 ) ) ;
#7129 = VERTEX_POINT ( 'NONE', #8933 ) ;
#7130 = CARTESIAN_POINT ( 'NONE',  ( 15.95292532278785913, -50.11873716947361856, 13.99999999999999822 ) ) ;
#7131 = DIRECTION ( 'NONE',  ( 0.000000000000000000, 0.000000000000000000, 1.000000000000000000 ) ) ;
#7132 = DIRECTION ( 'NONE',  ( -0.000000000000000000, -1.000000000000000000, -0.000000000000000000 ) ) ;
#7133 = DIRECTION ( 'NONE',  ( 0.000000000000000000, 1.000000000000000000, 0.000000000000000000 ) ) ;
#7134 = AXIS2_PLACEMENT_3D ( 'NONE', #17498, #13793, #3740 ) ;
#7135 = VERTEX_POINT ( 'NONE', #12368 ) ;
#7136 = DIRECTION ( 'NONE',  ( 0.000000000000000000, 0.000000000000000000, 1.000000000000000000 ) ) ;
#7137 = AXIS2_PLACEMENT_3D ( 'NONE', #12613, #7951, #11272 ) ;
#7138 = ORIENTED_EDGE ( 'NONE', *, *, #6102, .F. ) ;
#7139 = DIRECTION ( 'NONE',  ( 1.000000000000000000, 0.000000000000000000, 0.000000000000000000 ) ) ;
#7140 = DIRECTION ( 'NONE',  ( 1.000000000000000000, 0.000000000000000000, -0.000000000000000000 ) ) ;
#7141 = PRODUCT_DEFINITION ( 'UNKNOWN', '', #12987, #16911 ) ;
#7142 = ADVANCED_FACE ( 'NONE', ( #5707 ), #17539, .T. ) ;
#7143 = CARTESIAN_POINT ( 'NONE',  ( -15.21174975910705207, 41.81054587065082728, 13.75000000000000000 ) ) ;
#7144 = DIRECTION ( 'NONE',  ( -1.000000000000000000, 0.000000000000000000, 0.000000000000000000 ) ) ;
#7145 = VERTEX_POINT ( 'NONE', #2429 ) ;
#7146 = FACE_OUTER_BOUND ( 'NONE', #6027, .T. ) ;
#7147 = CARTESIAN_POINT ( 'NONE',  ( -25.37540678000426908, 38.74634676501045760, 42.50000000000000000 ) ) ;
#7148 = CARTESIAN_POINT ( 'NONE',  ( -23.61959064016851073, 45.26242829375641463, 68.50000000000000000 ) ) ;
#7149 = DIRECTION ( 'NONE',  ( -0.000000000000000000, -0.000000000000000000, -1.000000000000000000 ) ) ;
#7150 = ORIENTED_EDGE ( 'NONE', *, *, #5003, .F. ) ;
#7151 = CARTESIAN_POINT ( 'NONE',  ( -1.824728116533986810, 43.26054587065083012, 45.66679706732590205 ) ) ;
#7152 = EDGE_CURVE ( 'NONE', #17715, #19005, #16228, .T. ) ;
#7153 = ORIENTED_EDGE ( 'NONE', *, *, #4802, .T. ) ;
#7154 = TOROIDAL_SURFACE ( 'NONE', #11770, 1.500000000000000000, 0.5000000000000000000 ) ;
#7155 = CARTESIAN_POINT ( 'NONE',  ( -1.724728116533986721, 42.36054587065083155, 33.76679706732591058 ) ) ;
#7156 = AXIS2_PLACEMENT_3D ( 'NONE', #11294, #18127, #9642 ) ;
#7157 = CARTESIAN_POINT ( 'NONE',  ( 0.000000000000000000, 42.31054587065082728, 41.71679706732590631 ) ) ;
#7158 = VERTEX_POINT ( 'NONE', #19225 ) ;
#7159 = ORIENTED_EDGE ( 'NONE', *, *, #12375, .F. ) ;
#7160 = CARTESIAN_POINT ( 'NONE',  ( 1.774728116533979883, 42.36054587065083155, 49.66679706732590915 ) ) ;
#7161 = ORIENTED_EDGE ( 'NONE', *, *, #19688, .T. ) ;
#7162 = ORIENTED_EDGE ( 'NONE', *, *, #356, .F. ) ;
#7163 = CIRCLE ( 'NONE', #6, 0.2500000000000002220 ) ;
#7164 = VECTOR ( 'NONE', #3332, 1000.000000000000000 ) ;
#7165 = EDGE_LOOP ( 'NONE', ( #19908, #14133, #11643, #9057 ) ) ;
#7166 = CARTESIAN_POINT ( 'NONE',  ( 1.774728116533979883, 43.26054587065083012, 53.66679706732590915 ) ) ;
#7167 = CYLINDRICAL_SURFACE ( 'NONE', #1055, 0.1000000000000028644 ) ;
#7168 = DIRECTION ( 'NONE',  ( -0.000000000000000000, -0.000000000000000000, -1.000000000000000000 ) ) ;
#7169 = DIRECTION ( 'NONE',  ( -1.000000000000000000, 0.000000000000000000, 0.000000000000000000 ) ) ;
#7170 = DIRECTION ( 'NONE',  ( 0.000000000000000000, 0.000000000000000000, 1.000000000000000000 ) ) ;
#7171 = UNCERTAINTY_MEASURE_WITH_UNIT (LENGTH_MEASURE( 1.000000000000000082E-05 ), #245, 'distance_accuracy_value', 'NONE');
#7172 = VERTEX_POINT ( 'NONE', #7155 ) ;
#7173 = CARTESIAN_POINT ( 'NONE',  ( -32.47706987357030073, 83.66206381164208494, 68.25000000000000000 ) ) ;
#7174 = EDGE_CURVE ( 'NONE', #814, #3057, #14093, .T. ) ;
#7175 = FACE_OUTER_BOUND ( 'NONE', #6108, .T. ) ;
#7176 = EDGE_CURVE ( 'NONE', #13135, #18406, #3904, .T. ) ;
#7177 = CARTESIAN_POINT ( 'NONE',  ( -1.824728116533986810, 42.36054587065083155, 51.70876104995653577 ) ) ;
#7178 = ORIENTED_EDGE ( 'NONE', *, *, #13134, .F. ) ;
#7179 = CARTESIAN_POINT ( 'NONE',  ( -1.724728116533986721, 42.36054587065083155, 31.80876104995653719 ) ) ;
#7180 = CARTESIAN_POINT ( 'NONE',  ( -1.724728116533986721, 43.31054587065082728, 45.66679706732590205 ) ) ;
#7181 = ORIENTED_EDGE ( 'NONE', *, *, #13869, .T. ) ;
#7182 = ORIENTED_EDGE ( 'NONE', *, *, #17279, .T. ) ;
#7183 = DIRECTION ( 'NONE',  ( 0.000000000000000000, -0.000000000000000000, -1.000000000000000000 ) ) ;
#7184 = EDGE_CURVE ( 'NONE', #6576, #8378, #7589, .T. ) ;
#7185 = DIRECTION ( 'NONE',  ( 0.000000000000000000, 0.000000000000000000, 0.9999999999999998890 ) ) ;
#7186 = ORIENTED_EDGE ( 'NONE', *, *, #16575, .T. ) ;
#7187 = ADVANCED_FACE ( 'NONE', ( #2095 ), #17748, .T. ) ;
#7188 = CARTESIAN_POINT ( 'NONE',  ( -14.96174975910705207, -51.86873716947361856, 14.00000000000000000 ) ) ;
#7189 = ORIENTED_EDGE ( 'NONE', *, *, #14119, .T. ) ;
#7190 = ORIENTED_EDGE ( 'NONE', *, *, #15438, .F. ) ;
#7191 = CARTESIAN_POINT ( 'NONE',  ( -32.20000000000001705, -71.00000000000001421, 3.500000000000000000 ) ) ;
#7192 = DIRECTION ( 'NONE',  ( 0.000000000000000000, 0.000000000000000000, 1.000000000000000000 ) ) ;
#7193 = CARTESIAN_POINT ( 'NONE',  ( 1.724728116533979616, 42.36054587065083155, 51.70876104995653577 ) ) ;
#7194 = DIRECTION ( 'NONE',  ( -0.000000000000000000, -0.000000000000000000, -1.000000000000000000 ) ) ;
#7195 = CIRCLE ( 'NONE', #21142, 2.076718556943725424 ) ;
#7196 = CARTESIAN_POINT ( 'NONE',  ( 15.21174975910707161, -41.81054587065082728, 68.25000000000000000 ) ) ;
#7197 = EDGE_CURVE ( 'NONE', #11729, #12570, #11591, .T. ) ;
#7198 = PLANE ( 'NONE',  #18682 ) ;
#7199 = EDGE_CURVE ( 'NONE', #1525, #8484, #10826, .T. ) ;
#7200 = CARTESIAN_POINT ( 'NONE',  ( 15.21174975910707161, 51.86873716947361856, 68.00000000000000000 ) ) ;
#7201 = LINE ( 'NONE', #20741, #4105 ) ;
#7202 = DIRECTION ( 'NONE',  ( 1.000000000000000000, 0.000000000000000000, 0.000000000000000000 ) ) ;
#7203 = EDGE_CURVE ( 'NONE', #2930, #1905, #5914, .T. ) ;
#7204 = CIRCLE ( 'NONE', #21555, 0.1000000000000028644 ) ;
#7205 = DIRECTION ( 'NONE',  ( 0.000000000000000000, 0.000000000000000000, 1.000000000000000000 ) ) ;
#7206 = ORIENTED_EDGE ( 'NONE', *, *, #9926, .F. ) ;
#7207 = ORIENTED_EDGE ( 'NONE', *, *, #18196, .F. ) ;
#7208 = CARTESIAN_POINT ( 'NONE',  ( -25.37540678000429040, -36.74634676501047181, 13.79999999999999893 ) ) ;
#7209 =( LENGTH_UNIT ( ) NAMED_UNIT ( * ) SI_UNIT ( .MILLI., .METRE. ) );
#7210 = DIRECTION ( 'NONE',  ( 1.224646799147353207E-16, 0.000000000000000000, 1.000000000000000000 ) ) ;
#7211 = AXIS2_PLACEMENT_3D ( 'NONE', #8360, #15170, #10382 ) ;
#7212 = ORIENTED_EDGE ( 'NONE', *, *, #9646, .F. ) ;
#7213 = ORIENTED_EDGE ( 'NONE', *, *, #2106, .F. ) ;
#7214 = EDGE_CURVE ( 'NONE', #9565, #21823, #2207, .T. ) ;
#7215 = AXIS2_PLACEMENT_3D ( 'NONE', #14120, #19297, #3741 ) ;
#7216 = CIRCLE ( 'NONE', #5429, 0.2999999999999999334 ) ;
#7217 = CARTESIAN_POINT ( 'NONE',  ( -31.50000000000002132, 71.70000000000001705, 1.800000000000000044 ) ) ;
#7218 = AXIS2_PLACEMENT_3D ( 'NONE', #18917, #16889, #18681 ) ;
#7219 = LINE ( 'NONE', #17698, #1652 ) ;
#7220 = VERTEX_POINT ( 'NONE', #8519 ) ;
#7221 = CARTESIAN_POINT ( 'NONE',  ( 15.95292532278785913, 32.11873716947361856, 68.00000000000000000 ) ) ;
#7222 = CARTESIAN_POINT ( 'NONE',  ( -30.07540678000427548, -63.74634676501045050, 7.200000000000000178 ) ) ;
#7223 = DIRECTION ( 'NONE',  ( 0.000000000000000000, 0.000000000000000000, 1.000000000000000000 ) ) ;
#7224 = ADVANCED_FACE ( 'NONE', ( #12484 ), #17637, .T. ) ;
#7225 = CARTESIAN_POINT ( 'NONE',  ( 29.50000000000002132, 2.512390033608338236, 0.2999999999999947153 ) ) ;
#7226 = CARTESIAN_POINT ( 'NONE',  ( -15.05469906388004020, 52.39333383871511529, 13.50000000000000355 ) ) ;
#7227 = DIRECTION ( 'NONE',  ( -1.000000000000000000, -0.000000000000000000, 0.000000000000000000 ) ) ;
#7228 = EDGE_CURVE ( 'NONE', #1830, #879, #21134, .T. ) ;
#7229 = DIRECTION ( 'NONE',  ( -0.000000000000000000, -1.000000000000000000, -0.000000000000000000 ) ) ;
#7230 = CARTESIAN_POINT ( 'NONE',  ( -29.13662752439705272, 0.000000000000000000, 7.200000000000000178 ) ) ;
#7231 = DIRECTION ( 'NONE',  ( 0.000000000000000000, 0.000000000000000000, 1.000000000000000000 ) ) ;
#7232 = ORIENTED_EDGE ( 'NONE', *, *, #8962, .T. ) ;
#7233 = VECTOR ( 'NONE', #9029, 1000.000000000000000 ) ;
#7234 = ORIENTED_EDGE ( 'NONE', *, *, #13157, .F. ) ;
#7235 = EDGE_LOOP ( 'NONE', ( #21059, #10505, #4265, #14041 ) ) ;
#7236 = CARTESIAN_POINT ( 'NONE',  ( -15.95292532278785913, 34.11873716947361856, 42.50000000000000711 ) ) ;
#7237 = CYLINDRICAL_SURFACE ( 'NONE', #14922, 0.2500000000000002220 ) ;
#7238 = PLANE ( 'NONE',  #21816 ) ;
#7239 = ORIENTED_EDGE ( 'NONE', *, *, #6768, .F. ) ;
#7240 = VECTOR ( 'NONE', #21700, 1000.000000000000000 ) ;
#7241 = CARTESIAN_POINT ( 'NONE',  ( -9.178906393579156386, 42.46645089659917716, 70.50000000000000000 ) ) ;
#7242 = ORIENTED_EDGE ( 'NONE', *, *, #13073, .F. ) ;
#7243 = PLANE ( 'NONE',  #21513 ) ;
#7244 = ADVANCED_FACE ( 'NONE', ( #19663 ), #14484, .F. ) ;
#7245 = ORIENTED_EDGE ( 'NONE', *, *, #7078, .F. ) ;
#7246 = CARTESIAN_POINT ( 'NONE',  ( -30.19999999999999574, 69.70000000000001705, 1.500000000000000222 ) ) ;
#7247 = EDGE_CURVE ( 'NONE', #19749, #8671, #19118, .T. ) ;
#7248 = CARTESIAN_POINT ( 'NONE',  ( 30.67540678000428045, 6.000000000000000000, 3.799999999999999822 ) ) ;
#7249 = CARTESIAN_POINT ( 'NONE',  ( 33.79999999999999005, 84.70000000000001705, 78.20000000000000284 ) ) ;
#7250 = DIRECTION ( 'NONE',  ( -1.000000000000000000, 0.000000000000000000, 0.000000000000000000 ) ) ;
#7251 = ORIENTED_EDGE ( 'NONE', *, *, #8939, .T. ) ;
#7252 = CARTESIAN_POINT ( 'NONE',  ( 29.37540678000427619, 5.000000000000000000, 3.799999999999999822 ) ) ;
#7253 = DIRECTION ( 'NONE',  ( 1.000000000000000000, 0.000000000000000000, -0.000000000000000000 ) ) ;
#7254 = AXIS2_PLACEMENT_3D ( 'NONE', #21259, #7843, #16435 ) ;
#7255 = AXIS2_PLACEMENT_3D ( 'NONE', #1612, #8453, #6798 ) ;
#7256 = LINE ( 'NONE', #17853, #21779 ) ;
#7257 = VERTEX_POINT ( 'NONE', #6028 ) ;
#7258 = FACE_OUTER_BOUND ( 'NONE', #14678, .T. ) ;
#7259 = EDGE_CURVE ( 'NONE', #20751, #16560, #8398, .T. ) ;
#7260 = ORIENTED_EDGE ( 'NONE', *, *, #4116, .F. ) ;
#7261 = CARTESIAN_POINT ( 'NONE',  ( 0.000000000000000000, -32.61873716947361856, 68.00000000000000000 ) ) ;
#7262 = LINE ( 'NONE', #7043, #14140 ) ;
#7263 = EDGE_LOOP ( 'NONE', ( #18038, #10851, #20566, #9489 ) ) ;
#7264 = ORIENTED_EDGE ( 'NONE', *, *, #3785, .T. ) ;
#7265 = CIRCLE ( 'NONE', #14372, 0.2999999999999999334 ) ;
#7266 = CARTESIAN_POINT ( 'NONE',  ( -18.22752199202934520, 0.000000000000000000, 13.79999999999999893 ) ) ;
#7267 = FACE_OUTER_BOUND ( 'NONE', #7677, .T. ) ;
#7268 = ORIENTED_EDGE ( 'NONE', *, *, #16193, .F. ) ;
#7269 = VERTEX_POINT ( 'NONE', #4669 ) ;
#7270 = DIRECTION ( 'NONE',  ( 0.000000000000000000, 0.000000000000000000, 1.000000000000000000 ) ) ;
#7271 = CARTESIAN_POINT ( 'NONE',  ( -19.85144383993102934, 42.46645089659918426, 68.50000000000000000 ) ) ;
#7272 = ADVANCED_BREP_SHAPE_REPRESENTATION ( '', ( #5987, #17493 ), #3707 ) ;
#7273 = EDGE_CURVE ( 'NONE', #9408, #16887, #4466, .T. ) ;
#7274 = FACE_OUTER_BOUND ( 'NONE', #12277, .T. ) ;
#7275 = DIRECTION ( 'NONE',  ( 0.000000000000000000, 0.000000000000000000, -1.000000000000000000 ) ) ;
#7276 = CARTESIAN_POINT ( 'NONE',  ( -28.57540678000427548, 63.74634676501045050, 13.19999999999999929 ) ) ;
#7277 = DIRECTION ( 'NONE',  ( 1.000000000000000000, 0.000000000000000000, 0.000000000000000000 ) ) ;
#7278 = ORIENTED_EDGE ( 'NONE', *, *, #5587, .T. ) ;
#7279 = CARTESIAN_POINT ( 'NONE',  ( -24.00488095381848197, 42.46645089659918426, 68.25000000000000000 ) ) ;
#7280 = DIRECTION ( 'NONE',  ( 0.000000000000000000, 0.000000000000000000, 1.000000000000000000 ) ) ;
#7281 = DIRECTION ( 'NONE',  ( -8.673617379884034239E-17, -0.000000000000000000, 1.000000000000000000 ) ) ;
#7282 = ORIENTED_EDGE ( 'NONE', *, *, #14980, .T. ) ;
#7283 = DIRECTION ( 'NONE',  ( 1.000000000000000000, 0.000000000000000000, 0.000000000000000000 ) ) ;
#7284 = VERTEX_POINT ( 'NONE', #16167 ) ;
#7285 = EDGE_CURVE ( 'NONE', #17156, #1516, #2881, .T. ) ;
#7286 = ORIENTED_EDGE ( 'NONE', *, *, #4807, .T. ) ;
#7287 = CARTESIAN_POINT ( 'NONE',  ( 9.641460742840918030, 33.43424481021354921, 68.00000000000000000 ) ) ;
#7288 = PRODUCT_CONTEXT ( 'NONE', #3150, 'mechanical' ) ;
#7289 = ORIENTED_EDGE ( 'NONE', *, *, #6811, .F. ) ;
#7290 = ORIENTED_EDGE ( 'NONE', *, *, #15515, .T. ) ;
#7291 = ADVANCED_FACE ( 'NONE', ( #7815 ), #9594, .T. ) ;
#7292 = ADVANCED_FACE ( 'NONE', ( #958 ), #4224, .T. ) ;
#7293 = CARTESIAN_POINT ( 'NONE',  ( 23.02398829872513986, -3.528912754968635213, 13.79999999999999893 ) ) ;
#7294 = ORIENTED_EDGE ( 'NONE', *, *, #8160, .F. ) ;
#7295 = ORIENTED_EDGE ( 'NONE', *, *, #10767, .T. ) ;
#7296 = CARTESIAN_POINT ( 'NONE',  ( -1.724728116533986721, 43.26054587065083012, 49.76679706732591058 ) ) ;
#7297 = DIRECTION ( 'NONE',  ( 1.000000000000000000, -0.000000000000000000, -0.000000000000000000 ) ) ;
#7298 = CIRCLE ( 'NONE', #9428, 0.2500000000000002220 ) ;
#7299 =( NAMED_UNIT ( * ) SI_UNIT ( $, .STERADIAN. ) SOLID_ANGLE_UNIT ( ) );
#7300 = DIRECTION ( 'NONE',  ( 0.8556185176499236933, 0.5176069476490314791, 0.000000000000000000 ) ) ;
#7301 = CARTESIAN_POINT ( 'NONE',  ( 30.37540678000427619, 0.000000000000000000, 7.500000000000000000 ) ) ;
#7302 = DIRECTION ( 'NONE',  ( 0.000000000000000000, 0.000000000000000000, 1.000000000000000000 ) ) ;
#7303 = CIRCLE ( 'NONE', #17649, 0.2999999999999999334 ) ;
#7304 = FACE_OUTER_BOUND ( 'NONE', #10010, .T. ) ;
#7305 = CARTESIAN_POINT ( 'NONE',  ( -1.774728116533986544, 42.31054587065082728, 35.80876104995653009 ) ) ;
#7306 = CARTESIAN_POINT ( 'NONE',  ( -10.20831163238817574, 43.00645089659918341, 70.88527860057354246 ) ) ;
#7307 = DIRECTION ( 'NONE',  ( 1.000000000000000000, 0.000000000000000000, 0.000000000000000000 ) ) ;
#7308 = EDGE_CURVE ( 'NONE', #2242, #1813, #17969, .T. ) ;
#7309 = DIRECTION ( 'NONE',  ( 1.000000000000000000, -0.000000000000000000, -0.000000000000000000 ) ) ;
#7310 = VERTEX_POINT ( 'NONE', #9707 ) ;
#7311 = ORIENTED_EDGE ( 'NONE', *, *, #757, .F. ) ;
#7312 = CARTESIAN_POINT ( 'NONE',  ( -26.37540678000427619, 10.94079601157914539, 13.79999999999999893 ) ) ;
#7313 = SURFACE_STYLE_FILL_AREA ( #9315 ) ;
#7314 = CARTESIAN_POINT ( 'NONE',  ( -26.63662752439704917, -3.061616997868386099E-16, -18.50000000000000000 ) ) ;
#7315 = ORIENTED_EDGE ( 'NONE', *, *, #13726, .F. ) ;
#7316 = B_SPLINE_CURVE_WITH_KNOTS ( 'NONE', 3,
 ( #9221, #14576, #17707, #14354, #1042, #21429, #19737, #705, #19845, #7554 ),
 .UNSPECIFIED., .F., .F.,
 ( 4, 2, 2, 2, 4 ),
 ( 0.000000000000000000, 0.0007882085451459019303, 0.001182312817718852950, 0.001379364954005326887, 0.001576417090291801042 ),
 .UNSPECIFIED. ) ;
#7317 = EDGE_LOOP ( 'NONE', ( #21156, #4801, #922, #17153 ) ) ;
#7318 = ORIENTED_EDGE ( 'NONE', *, *, #9780, .T. ) ;
#7319 = EDGE_CURVE ( 'NONE', #6172, #13182, #18782, .T. ) ;
#7320 = EDGE_CURVE ( 'NONE', #8703, #1886, #17327, .T. ) ;
#7321 = VECTOR ( 'NONE', #11751, 1000.000000000000000 ) ;
#7322 = FACE_OUTER_BOUND ( 'NONE', #15277, .T. ) ;
#7323 = DIRECTION ( 'NONE',  ( 0.000000000000000000, 0.000000000000000000, -1.000000000000000000 ) ) ;
#7324 = ORIENTED_EDGE ( 'NONE', *, *, #12217, .T. ) ;
#7325 = DIRECTION ( 'NONE',  ( -0.2309407893632008379, 0.9729678061520339316, 0.000000000000000000 ) ) ;
#7326 = DIRECTION ( 'NONE',  ( 1.000000000000000000, 2.832483164223434527E-16, -0.000000000000000000 ) ) ;
#7327 = CARTESIAN_POINT ( 'NONE',  ( 1.774728116533979438, 43.31054587065082728, 51.80876104995653719 ) ) ;
#7328 = CARTESIAN_POINT ( 'NONE',  ( 29.37540678000427619, 6.000000000000000000, 3.500000000000000000 ) ) ;
#7329 = DIRECTION ( 'NONE',  ( 0.000000000000000000, 0.000000000000000000, 1.000000000000000000 ) ) ;
#7330 = DIRECTION ( 'NONE',  ( 1.000000000000000000, 0.000000000000000000, 0.000000000000000000 ) ) ;
#7331 = EDGE_CURVE ( 'NONE', #22136, #13456, #22001, .T. ) ;
#7332 = FACE_OUTER_BOUND ( 'NONE', #4804, .T. ) ;
#7333 = CARTESIAN_POINT ( 'NONE',  ( -21.92816239687475743, 42.46645089659918426, 68.25000000000000000 ) ) ;
#7334 = DIRECTION ( 'NONE',  ( 1.000000000000000000, 0.000000000000000000, 0.000000000000000000 ) ) ;
#7335 = VERTEX_POINT ( 'NONE', #21680 ) ;
#7336 = ORIENTED_EDGE ( 'NONE', *, *, #3701, .F. ) ;
#7337 = AXIS2_PLACEMENT_3D ( 'NONE', #9310, #14430, #21283 ) ;
#7338 = VERTEX_POINT ( 'NONE', #11369 ) ;
#7339 = DIRECTION ( 'NONE',  ( -1.000000000000000000, 0.000000000000000000, 0.000000000000000000 ) ) ;
#7340 = CARTESIAN_POINT ( 'NONE',  ( -25.37540678000427263, 63.74634676501045050, 3.799999999999999822 ) ) ;
#7341 = ORIENTED_EDGE ( 'NONE', *, *, #15873, .T. ) ;
#7342 = DIRECTION ( 'NONE',  ( -0.000000000000000000, 1.000000000000000000, -0.000000000000000000 ) ) ;
#7343 = EDGE_CURVE ( 'NONE', #7220, #3984, #18418, .T. ) ;
#7344 = EDGE_CURVE ( 'NONE', #1486, #17848, #18198, .T. ) ;
#7345 = ORIENTED_EDGE ( 'NONE', *, *, #17304, .F. ) ;
#7346 = DIRECTION ( 'NONE',  ( 1.000000000000000000, 0.000000000000000000, 0.000000000000000000 ) ) ;
#7347 = DIRECTION ( 'NONE',  ( 1.000000000000000000, 0.000000000000000000, 0.000000000000000000 ) ) ;
#7348 = EDGE_CURVE ( 'NONE', #14892, #1748, #8022, .T. ) ;
#7349 = VERTEX_POINT ( 'NONE', #16608 ) ;
#7350 = FACE_OUTER_BOUND ( 'NONE', #273, .T. ) ;
#7351 = DIRECTION ( 'NONE',  ( 1.000000000000000000, 0.000000000000000000, 0.000000000000000000 ) ) ;
#7352 = CIRCLE ( 'NONE', #10208, 2.500000000000002220 ) ;
#7353 = CARTESIAN_POINT ( 'NONE',  ( -21.92816239687475743, 42.46645089659918426, 13.74999999999999822 ) ) ;
#7354 = CIRCLE ( 'NONE', #13407, 0.2999999999999999334 ) ;
#7355 = CARTESIAN_POINT ( 'NONE',  ( -1.724728116533986721, 42.36054587065083155, 33.66679706732590915 ) ) ;
#7356 = EDGE_LOOP ( 'NONE', ( #3008, #21874, #545, #3971 ) ) ;
#7357 = DIRECTION ( 'NONE',  ( 0.000000000000000000, 0.000000000000000000, 1.000000000000000000 ) ) ;
#7358 = DIRECTION ( 'NONE',  ( 0.000000000000000000, 0.000000000000000000, 1.000000000000000000 ) ) ;
#7359 = CARTESIAN_POINT ( 'NONE',  ( -1.774728116533986766, 42.36054587065083155, 47.80876104995653719 ) ) ;
#7360 = DIRECTION ( 'NONE',  ( 0.000000000000000000, 0.000000000000000000, -1.000000000000000000 ) ) ;
#7361 = ORIENTED_EDGE ( 'NONE', *, *, #8723, .T. ) ;
#7362 = VERTEX_POINT ( 'NONE', #21236 ) ;
#7363 = DIRECTION ( 'NONE',  ( 0.000000000000000000, 0.000000000000000000, -1.000000000000000000 ) ) ;
#7364 = CARTESIAN_POINT ( 'NONE',  ( -28.87540678000427619, -6.494748934539263274, 13.19999999999999929 ) ) ;
#7365 = ORIENTED_EDGE ( 'NONE', *, *, #2373, .T. ) ;
#7366 = VECTOR ( 'NONE', #2562, 1000.000000000000000 ) ;
#7367 = ORIENTED_EDGE ( 'NONE', *, *, #13784, .T. ) ;
#7368 = FACE_OUTER_BOUND ( 'NONE', #17362, .T. ) ;
#7369 = ADVANCED_FACE ( 'NONE', ( #1175 ), #4434, .T. ) ;
#7370 = LINE ( 'NONE', #14170, #17429 ) ;
#7371 = AXIS2_PLACEMENT_3D ( 'NONE', #10859, #17674, #3711 ) ;
#7372 = ORIENTED_EDGE ( 'NONE', *, *, #19365, .F. ) ;
#7373 = AXIS2_PLACEMENT_3D ( 'NONE', #14025, #478, #11005 ) ;
#7374 = AXIS2_PLACEMENT_3D ( 'NONE', #18393, #12914, #7676 ) ;
#7375 = ORIENTED_EDGE ( 'NONE', *, *, #9074, .T. ) ;
#7376 = EDGE_CURVE ( 'NONE', #17182, #14452, #190, .T. ) ;
#7377 = ORIENTED_EDGE ( 'NONE', *, *, #6149, .T. ) ;
#7378 = DIRECTION ( 'NONE',  ( -0.000000000000000000, 0.000000000000000000, 1.000000000000000000 ) ) ;
#7379 = VECTOR ( 'NONE', #2020, 1000.000000000000000 ) ;
#7380 = VECTOR ( 'NONE', #8377, 1000.000000000000000 ) ;
#7381 = CIRCLE ( 'NONE', #17699, 0.2999999999999999334 ) ;
#7382 = CARTESIAN_POINT ( 'NONE',  ( -11.62890639357915923, 41.92645089659917801, 70.88527860057354246 ) ) ;
#7383 = LINE ( 'NONE', #10622, #9939 ) ;
#7384 = ORIENTED_EDGE ( 'NONE', *, *, #12466, .F. ) ;
#7385 = CARTESIAN_POINT ( 'NONE',  ( 14.71479891163412113, 52.07369784467161367, 13.50000000000000000 ) ) ;
#7386 = DIRECTION ( 'NONE',  ( 0.000000000000000000, 0.000000000000000000, 1.000000000000000000 ) ) ;
#7387 = DIRECTION ( 'NONE',  ( 0.000000000000000000, 1.000000000000000000, 0.000000000000000000 ) ) ;
#7388 = EDGE_LOOP ( 'NONE', ( #15263, #19459, #6723, #17887 ) ) ;
#7389 = EDGE_CURVE ( 'NONE', #20601, #3171, #7803, .T. ) ;
#7390 = DIRECTION ( 'NONE',  ( 0.000000000000000000, 1.000000000000000000, 0.000000000000000000 ) ) ;
#7391 = ORIENTED_EDGE ( 'NONE', *, *, #12503, .T. ) ;
#7392 = ADVANCED_FACE ( 'NONE', ( #10035 ), #18865, .F. ) ;
#7393 = AXIS2_PLACEMENT_3D ( 'NONE', #496, #6950, #105 ) ;
#7394 = AXIS2_PLACEMENT_3D ( 'NONE', #22119, #18970, #10240 ) ;
#7395 = AXIS2_PLACEMENT_3D ( 'NONE', #12486, #2643, #19883 ) ;
#7396 = EDGE_LOOP ( 'NONE', ( #11012, #15796, #540, #8434, #21317, #2191, #18209, #21859, #18582, #19553 ) ) ;
#7397 = AXIS2_PLACEMENT_3D ( 'NONE', #18088, #1190, #13045 ) ;
#7398 = DIRECTION ( 'NONE',  ( -0.000000000000000000, -0.000000000000000000, -1.000000000000000000 ) ) ;
#7399 = ITEM_DEFINED_TRANSFORMATION ( 'NONE', 'NONE', #1918,  #17493 ) ;
#7400 = ORIENTED_EDGE ( 'NONE', *, *, #5879, .F. ) ;
#7401 = VERTEX_POINT ( 'NONE', #10251 ) ;
#7402 = CIRCLE ( 'NONE', #19914, 1.750000000000001554 ) ;
#7403 = CARTESIAN_POINT ( 'NONE',  ( 23.02398829872513986, -2.558598175897759841, 13.47089014135852914 ) ) ;
#7404 = VERTEX_POINT ( 'NONE', #18525 ) ;
#7405 = DIRECTION ( 'NONE',  ( 1.000000000000000000, 0.000000000000000000, 0.000000000000000000 ) ) ;
#7406 = ORIENTED_EDGE ( 'NONE', *, *, #12281, .F. ) ;
#7407 = DIRECTION ( 'NONE',  ( -0.000000000000000000, -1.000000000000000000, -0.000000000000000000 ) ) ;
#7408 = DIRECTION ( 'NONE',  ( 1.000000000000000000, 0.000000000000000000, -0.000000000000000000 ) ) ;
#7409 = DIRECTION ( 'NONE',  ( 0.000000000000000000, 0.000000000000000000, 1.000000000000000000 ) ) ;
#7410 = CIRCLE ( 'NONE', #10662, 3.500000000000003109 ) ;
#7411 = ADVANCED_FACE ( 'NONE', ( #20110 ), #6638, .T. ) ;
#7412 = TOROIDAL_SURFACE ( 'NONE', #19190, 3.800000000000002931, 0.2999999999999999889 ) ;
#7413 = AXIS2_PLACEMENT_3D ( 'NONE', #4722, #16556, #5880 ) ;
#7414 = CARTESIAN_POINT ( 'NONE',  ( -1.724728116533986721, 43.26054587065083012, 37.66679706732590915 ) ) ;
#7415 = AXIS2_PLACEMENT_3D ( 'NONE', #4690, #18326, #3001 ) ;
#7416 = CARTESIAN_POINT ( 'NONE',  ( 1.724728116533979616, 43.26054587065083012, 43.70876104995653577 ) ) ;
#7417 = AXIS2_PLACEMENT_3D ( 'NONE', #18723, #8225, #6561 ) ;
#7418 = DIRECTION ( 'NONE',  ( -2.832483164223434527E-16, 1.000000000000000000, 0.000000000000000000 ) ) ;
#7419 = DIRECTION ( 'NONE',  ( 0.000000000000000000, 1.000000000000000000, 0.000000000000000000 ) ) ;
#7420 = CIRCLE ( 'NONE', #19200, 0.1000000000000028644 ) ;
#7421 = CARTESIAN_POINT ( 'NONE',  ( -17.95292532278785913, -38.74634676501046471, 42.50000000000000711 ) ) ;
#7422 = EDGE_CURVE ( 'NONE', #9580, #18991, #8583, .T. ) ;
#7423 = ORIENTED_EDGE ( 'NONE', *, *, #6245, .T. ) ;
#7424 = ORIENTED_EDGE ( 'NONE', *, *, #2277, .F. ) ;
#7425 = CARTESIAN_POINT ( 'NONE',  ( 9.141460742840918030, -32.61873716947361856, 7.321391277662001151 ) ) ;
#7426 = ORIENTED_EDGE ( 'NONE', *, *, #1844, .F. ) ;
#7427 = EDGE_LOOP ( 'NONE', ( #8034, #14387, #15607, #1693 ) ) ;
#7428 = TOROIDAL_SURFACE ( 'NONE', #10988, 0.05000000000000000278, 0.05000000000000000278 ) ;
#7429 = AXIS2_PLACEMENT_3D ( 'NONE', #10523, #2003, #7512 ) ;
#7430 = ORIENTED_EDGE ( 'NONE', *, *, #2794, .T. ) ;
#7431 = CIRCLE ( 'NONE', #18866, 0.9652499999999990532 ) ;
#7432 = VECTOR ( 'NONE', #11779, 1000.000000000000000 ) ;
#7433 = ADVANCED_FACE ( 'NONE', ( #13486 ), #6915, .T. ) ;
#7434 = DIRECTION ( 'NONE',  ( 0.000000000000000000, 0.000000000000000000, -1.000000000000000000 ) ) ;
#7435 = DIRECTION ( 'NONE',  ( 0.000000000000000000, 0.000000000000000000, 1.000000000000000000 ) ) ;
#7436 = VERTEX_POINT ( 'NONE', #3314 ) ;
#7437 = FACE_OUTER_BOUND ( 'NONE', #18252, .T. ) ;
#7438 = CARTESIAN_POINT ( 'NONE',  ( -17.45292532278785913, 0.000000000000000000, 13.99999999999999822 ) ) ;
#7439 = SPHERICAL_SURFACE ( 'NONE', #21517, 0.2500000000000000000 ) ;
#7440 = CARTESIAN_POINT ( 'NONE',  ( 15.04770344846787822, 51.92604205163220854, 13.50000000000000000 ) ) ;
#7441 = CYLINDRICAL_SURFACE ( 'NONE', #4010, 0.05000000000000143219 ) ;
#7442 = VECTOR ( 'NONE', #13639, 1000.000000000000000 ) ;
#7443 = VECTOR ( 'NONE', #7673, 1000.000000000000000 ) ;
#7444 = AXIS2_PLACEMENT_3D ( 'NONE', #3575, #15316, #11833 ) ;
#7445 = CARTESIAN_POINT ( 'NONE',  ( 29.13662752439705272, 0.000000000000000000, 0.000000000000000000 ) ) ;
#7446 = EDGE_CURVE ( 'NONE', #22072, #16612, #20580, .T. ) ;
#7447 = EDGE_CURVE ( 'NONE', #11183, #4799, #15273, .T. ) ;
#7448 = CARTESIAN_POINT ( 'NONE',  ( -1.724728116533986721, 42.31054587065082728, 39.80876104995653719 ) ) ;
#7449 = FACE_OUTER_BOUND ( 'NONE', #3012, .T. ) ;
#7450 = ADVANCED_FACE ( 'NONE', ( #22006 ), #21901, .T. ) ;
#7451 = VECTOR ( 'NONE', #5045, 1000.000000000000000 ) ;
#7452 = CYLINDRICAL_SURFACE ( 'NONE', #2752, 0.2500000000000002220 ) ;
#7453 = ORIENTED_EDGE ( 'NONE', *, *, #3146, .T. ) ;
#7454 = ORIENTED_EDGE ( 'NONE', *, *, #17246, .T. ) ;
#7455 = AXIS2_PLACEMENT_3D ( 'NONE', #5529, #20852, #19059 ) ;
#7456 = ORIENTED_EDGE ( 'NONE', *, *, #21487, .F. ) ;
#7457 = CARTESIAN_POINT ( 'NONE',  ( 27.65375860907908745, -2.282443358843508019, -3.134021904840910022E-17 ) ) ;
#7458 = VECTOR ( 'NONE', #15934, 1000.000000000000000 ) ;
#7459 = CARTESIAN_POINT ( 'NONE',  ( 17.95292532278785913, -34.11873716947361856, 68.00000000000000000 ) ) ;
#7460 = ORIENTED_EDGE ( 'NONE', *, *, #20953, .T. ) ;
#7461 = SHAPE_REPRESENTATION ( 'Front Plate', ( #17493 ), #6222 ) ;
#7462 = CARTESIAN_POINT ( 'NONE',  ( 31.44597781366222122, 56.94165929845684104, 68.50000000000000000 ) ) ;
#7463 = ORIENTED_EDGE ( 'NONE', *, *, #3831, .F. ) ;
#7464 = DIRECTION ( 'NONE',  ( 1.000000000000000000, 0.000000000000000000, 0.000000000000000000 ) ) ;
#7465 = AXIS2_PLACEMENT_3D ( 'NONE', #13331, #16916, #4740 ) ;
#7466 = CARTESIAN_POINT ( 'NONE',  ( 14.71174975910707161, 51.86873716947361856, 68.00000000000000000 ) ) ;
#7467 = EDGE_CURVE ( 'NONE', #2970, #20337, #14458, .T. ) ;
#7468 = ORIENTED_EDGE ( 'NONE', *, *, #202, .T. ) ;
#7469 = DIRECTION ( 'NONE',  ( 0.000000000000000000, 0.000000000000000000, -1.000000000000000000 ) ) ;
#7470 = CARTESIAN_POINT ( 'NONE',  ( 32.50000000000002132, 72.00000000000001421, 3.500000000000000000 ) ) ;
#7471 = CIRCLE ( 'NONE', #10327, 2.000000000000001776 ) ;
#7472 = CIRCLE ( 'NONE', #18847, 5.000000000000004441 ) ;
#7473 = DIRECTION ( 'NONE',  ( 1.000000000000000000, 0.000000000000000000, 0.000000000000000000 ) ) ;
#7474 = CIRCLE ( 'NONE', #14584, 1.999999999999991340 ) ;
#7475 = ORIENTED_EDGE ( 'NONE', *, *, #2901, .T. ) ;
#7476 = CARTESIAN_POINT ( 'NONE',  ( -32.20000000000001705, 71.00000000000001421, 3.500000000000000000 ) ) ;
#7477 = AXIS2_PLACEMENT_3D ( 'NONE', #99, #6607, #14978 ) ;
#7478 = CARTESIAN_POINT ( 'NONE',  ( -1.724728116533986721, 43.26054587065083012, 37.76679706732590347 ) ) ;
#7479 = CARTESIAN_POINT ( 'NONE',  ( -8.641460742840918030, -32.93424481021354921, 68.00000000000000000 ) ) ;
#7480 = CARTESIAN_POINT ( 'NONE',  ( -28.87540678000427619, -63.74634676501045050, 13.19999999999999929 ) ) ;
#7481 = ORIENTED_EDGE ( 'NONE', *, *, #4560, .T. ) ;
#7482 = DIRECTION ( 'NONE',  ( 0.000000000000000000, 1.000000000000000000, 0.000000000000000000 ) ) ;
#7483 = ADVANCED_FACE ( 'NONE', ( #8136 ), #14944, .T. ) ;
#7484 = ORIENTED_EDGE ( 'NONE', *, *, #10081, .T. ) ;
#7485 = DIRECTION ( 'NONE',  ( 0.000000000000000000, 0.000000000000000000, 1.000000000000000000 ) ) ;
#7486 = ADVANCED_FACE ( 'NONE', ( #15056 ), #20441, .F. ) ;
#7487 = LINE ( 'NONE', #512, #17697 ) ;
#7488 = CIRCLE ( 'NONE', #19989, 1.000000000000000888 ) ;
#7489 = ORIENTED_EDGE ( 'NONE', *, *, #14414, .T. ) ;
#7490 = ORIENTED_EDGE ( 'NONE', *, *, #2043, .F. ) ;
#7492 = ADVANCED_FACE ( 'NONE', ( #4774 ), #18747, .T. ) ;
#7491 = DIRECTION ( 'NONE',  ( 1.000000000000000000, 0.000000000000000000, 0.000000000000000000 ) ) ;
#7493 = CARTESIAN_POINT ( 'NONE',  ( 25.37540678000427263, 63.74634676501045050, 7.799999999999999822 ) ) ;
#7494 = AXIS2_PLACEMENT_3D ( 'NONE', #13592, #16831, #8450 ) ;
#7495 = ORIENTED_EDGE ( 'NONE', *, *, #10782, .F. ) ;
#7496 = AXIS2_PLACEMENT_3D ( 'NONE', #17225, #17561, #9059 ) ;
#7497 = ORIENTED_EDGE ( 'NONE', *, *, #4590, .T. ) ;
#7498 = EDGE_CURVE ( 'NONE', #17454, #13749, #6285, .T. ) ;
#7499 = CARTESIAN_POINT ( 'NONE',  ( 3.127054932750481964, -32.11873716947361856, 42.50000000000000711 ) ) ;
#7500 = CARTESIAN_POINT ( 'NONE',  ( -9.641460742840918030, -32.61873716947361856, 42.50000000000000711 ) ) ;
#7501 = DIRECTION ( 'NONE',  ( 1.301042606982568087E-14, 0.000000000000000000, 1.000000000000000000 ) ) ;
#7502 = DIRECTION ( 'NONE',  ( 0.000000000000000000, -1.000000000000000000, 0.000000000000000000 ) ) ;
#7503 = ADVANCED_FACE ( 'NONE', ( #11691 ), #12311, .F. ) ;
#7504 = DIRECTION ( 'NONE',  ( 1.301042606982568087E-14, 0.000000000000000000, 1.000000000000000000 ) ) ;
#7505 = DIRECTION ( 'NONE',  ( 1.000000000000000000, 0.000000000000000000, 0.000000000000000000 ) ) ;
#7506 = ORIENTED_EDGE ( 'NONE', *, *, #11521, .T. ) ;
#7507 = CARTESIAN_POINT ( 'NONE',  ( 1.774728116533979883, 43.26054587065083012, 49.66679706732590915 ) ) ;
#7508 = DIRECTION ( 'NONE',  ( -1.000000000000000000, 0.000000000000000000, 0.000000000000000000 ) ) ;
#7509 = DIRECTION ( 'NONE',  ( -0.000000000000000000, 1.000000000000000000, -0.000000000000000000 ) ) ;
#7510 = ADVANCED_FACE ( 'NONE', ( #8349 ), #5931, .T. ) ;
#7511 = ORIENTED_EDGE ( 'NONE', *, *, #8962, .F. ) ;
#7512 = DIRECTION ( 'NONE',  ( 0.000000000000000000, 0.000000000000000000, 1.000000000000000000 ) ) ;
#7513 = ORIENTED_EDGE ( 'NONE', *, *, #4260, .F. ) ;
#7514 = EDGE_LOOP ( 'NONE', ( #12855, #4920, #5843, #20909, #19702 ) ) ;
#7515 = ORIENTED_EDGE ( 'NONE', *, *, #16398, .T. ) ;
#7516 = CARTESIAN_POINT ( 'NONE',  ( 34.39999999999998437, -84.70000000000001705, 4.249524393041314059E-15 ) ) ;
#7517 = CIRCLE ( 'NONE', #2128, 0.3000000000000016542 ) ;
#7518 = ORIENTED_EDGE ( 'NONE', *, *, #11039, .F. ) ;
#7519 = VECTOR ( 'NONE', #16404, 1000.000000000000000 ) ;
#7520 = CIRCLE ( 'NONE', #1790, 0.5000000000000000000 ) ;
#7521 = EDGE_LOOP ( 'NONE', ( #21544, #7463, #21767, #4833 ) ) ;
#7522 = VERTEX_POINT ( 'NONE', #2060 ) ;
#7523 = DIRECTION ( 'NONE',  ( -0.000000000000000000, 1.000000000000000000, -0.000000000000000000 ) ) ;
#7524 = ORIENTED_EDGE ( 'NONE', *, *, #16883, .T. ) ;
#7525 = CARTESIAN_POINT ( 'NONE',  ( 33.79999999999999005, 85.00000000000000000, 78.20000000000000284 ) ) ;
#7526 = EDGE_CURVE ( 'NONE', #11236, #8930, #14110, .T. ) ;
#7527 = DIRECTION ( 'NONE',  ( 0.000000000000000000, 0.000000000000000000, 1.000000000000000000 ) ) ;
#7528 = FACE_OUTER_BOUND ( 'NONE', #16266, .T. ) ;
#7529 = ADVANCED_FACE ( 'NONE', ( #10471 ), #4835, .T. ) ;
#7530 = EDGE_CURVE ( 'NONE', #17106, #6358, #17611, .T. ) ;
#7531 = AXIS2_PLACEMENT_3D ( 'NONE', #6456, #1384, #6565 ) ;
#7532 = CIRCLE ( 'NONE', #5380, 0.5000000000000004441 ) ;
#7533 = CARTESIAN_POINT ( 'NONE',  ( 4.127054932750481520, 33.93424481021354921, 68.50000000000000000 ) ) ;
#7534 = CARTESIAN_POINT ( 'NONE',  ( 0.000000000000000000, 69.00000000000000000, -150.0833101980363722 ) ) ;
#7535 = DIRECTION ( 'NONE',  ( -2.832483164223434527E-16, -1.000000000000000000, -0.000000000000000000 ) ) ;
#7536 = CARTESIAN_POINT ( 'NONE',  ( 25.37540678000429395, -39.04634676501046187, 13.50000000000000000 ) ) ;
#7537 = DIRECTION ( 'NONE',  ( 0.000000000000000000, 0.000000000000000000, 1.000000000000000000 ) ) ;
#7538 = ORIENTED_EDGE ( 'NONE', *, *, #17275, .F. ) ;
#7539 = DIRECTION ( 'NONE',  ( 0.000000000000000000, 0.000000000000000000, 1.000000000000000000 ) ) ;
#7540 =( NAMED_UNIT ( * ) PLANE_ANGLE_UNIT ( ) SI_UNIT ( $, .RADIAN. ) );
#7541 = FACE_OUTER_BOUND ( 'NONE', #3319, .T. ) ;
#7542 = ORIENTED_EDGE ( 'NONE', *, *, #2273, .F. ) ;
#7543 = EDGE_LOOP ( 'NONE', ( #4421, #21053, #17891, #11528 ) ) ;
#7544 = VECTOR ( 'NONE', #21189, 999.9999999999998863 ) ;
#7545 = MECHANICAL_DESIGN_GEOMETRIC_PRESENTATION_REPRESENTATION (  '', ( #18599 ), #15023 ) ;
#7546 = EDGE_CURVE ( 'NONE', #9117, #19361, #17691, .T. ) ;
#7547 = CARTESIAN_POINT ( 'NONE',  ( 14.96174975910705918, 32.10873716947361345, 13.05380965755522737 ) ) ;
#7548 = ADVANCED_BREP_SHAPE_REPRESENTATION ( '', ( #6179, #17493 ), #10355 ) ;
#7549 = ADVANCED_FACE ( 'NONE', ( #15915 ), #13800, .F. ) ;
#7550 = EDGE_LOOP ( 'NONE', ( #20728, #13342, #19464, #2033 ) ) ;
#7551 = DIRECTION ( 'NONE',  ( -0.000000000000000000, -0.000000000000000000, -1.000000000000000000 ) ) ;
#7552 = DIRECTION ( 'NONE',  ( -1.000000000000000000, -0.000000000000000000, -0.000000000000000000 ) ) ;
#7553 = FACE_OUTER_BOUND ( 'NONE', #15169, .T. ) ;
#7554 = CARTESIAN_POINT ( 'NONE',  ( -23.02398829872513986, 2.157133568460765538, 13.19999999999999929 ) ) ;
#7555 = ORIENTED_EDGE ( 'NONE', *, *, #7530, .F. ) ;
#7556 = DIRECTION ( 'NONE',  ( 1.000000000000000000, 0.000000000000000000, 0.000000000000000000 ) ) ;
#7557 = AXIS2_PLACEMENT_3D ( 'NONE', #6621, #6519, #20150 ) ;
#7558 = DIRECTION ( 'NONE',  ( -1.000000000000000000, 0.000000000000000000, -6.123233995736764803E-17 ) ) ;
#7559 = CARTESIAN_POINT ( 'NONE',  ( -31.01761816434226660, 84.00847499568689614, 68.50000000000000000 ) ) ;
#7560 = ORIENTED_EDGE ( 'NONE', *, *, #11231, .F. ) ;
#7561 = ORIENTED_EDGE ( 'NONE', *, *, #10041, .F. ) ;
#7562 = CARTESIAN_POINT ( 'NONE',  ( 27.61238352468048518, -2.348761424523157615, 0.000000000000000000 ) ) ;
#7563 = CYLINDRICAL_SURFACE ( 'NONE', #1006, 0.05000000000000143219 ) ;
#7564 = EDGE_LOOP ( 'NONE', ( #9836, #15521, #5936, #5188 ) ) ;
#7565 = AXIS2_PLACEMENT_3D ( 'NONE', #20652, #10243, #5334 ) ;
#7566 = ADVANCED_FACE ( 'NONE', ( #20873 ), #3056, .T. ) ;
#7567 = CIRCLE ( 'NONE', #69, 0.2999999999999999889 ) ;
#7568 = PLANE ( 'NONE',  #15923 ) ;
#7569 = AXIS2_PLACEMENT_3D ( 'NONE', #1041, #16367, #14906 ) ;
#7570 = CIRCLE ( 'NONE', #21524, 0.2500000000000002220 ) ;
#7571 = EDGE_LOOP ( 'NONE', ( #13635, #16926, #22153, #20179 ) ) ;
#7572 = FACE_OUTER_BOUND ( 'NONE', #12006, .T. ) ;
#7573 = DIRECTION ( 'NONE',  ( 0.000000000000000000, 1.000000000000000000, 0.000000000000000000 ) ) ;
#7574 = ADVANCED_FACE ( 'NONE', ( #7449 ), #11975, .T. ) ;
#7575 = ADVANCED_FACE ( 'NONE', ( #5777 ), #17386, .F. ) ;
#7576 = FACE_OUTER_BOUND ( 'NONE', #11450, .T. ) ;
#7577 = DIRECTION ( 'NONE',  ( -1.000000000000000000, 0.000000000000000000, 0.000000000000000000 ) ) ;
#7578 = DIRECTION ( 'NONE',  ( -1.000000000000000000, 0.000000000000000000, 0.000000000000000000 ) ) ;
#7579 = DIRECTION ( 'NONE',  ( 0.000000000000000000, 0.000000000000000000, -1.000000000000000000 ) ) ;
#7580 = VERTEX_POINT ( 'NONE', #3980 ) ;
#7581 = DIRECTION ( 'NONE',  ( 2.107255972849994642E-16, -0.000000000000000000, 1.000000000000000000 ) ) ;
#7582 = DIRECTION ( 'NONE',  ( 1.000000000000000000, 0.000000000000000000, 0.000000000000000000 ) ) ;
#7583 = CARTESIAN_POINT ( 'NONE',  ( -34.70000000000000284, 84.70000000000001705, -6.019490461639519829E-15 ) ) ;
#7584 = FACE_OUTER_BOUND ( 'NONE', #19877, .T. ) ;
#7585 = EDGE_LOOP ( 'NONE', ( #13621, #21794, #6275, #9048 ) ) ;
#7586 = SURFACE_STYLE_FILL_AREA ( #6132 ) ;
#7587 = ORIENTED_EDGE ( 'NONE', *, *, #5906, .F. ) ;
#7588 = VECTOR ( 'NONE', #17339, 1000.000000000000000 ) ;
#7589 = LINE ( 'NONE', #1676, #8770 ) ;
#7590 = CIRCLE ( 'NONE', #12907, 2.767785046117004377 ) ;
#7591 = DIRECTION ( 'NONE',  ( 1.000000000000000000, 0.000000000000000000, -0.000000000000000000 ) ) ;
#7592 = EDGE_LOOP ( 'NONE', ( #2156, #21608, #672, #3318 ) ) ;
#7593 = AXIS2_PLACEMENT_3D ( 'NONE', #11792, #6907, #18738 ) ;
#7594 = EDGE_LOOP ( 'NONE', ( #19317, #20342, #10359, #12955 ) ) ;
#7595 = DIRECTION ( 'NONE',  ( 0.9729678061520313781, 0.2309407893632113573, 0.000000000000000000 ) ) ;
#7596 = ADVANCED_FACE ( 'NONE', ( #19406 ), #12129, .T. ) ;
#7597 = CARTESIAN_POINT ( 'NONE',  ( -1.774728116533986766, 42.36054587065083155, 53.66679706732590915 ) ) ;
#7598 = VERTEX_POINT ( 'NONE', #20980 ) ;
#7599 = VERTEX_POINT ( 'NONE', #20769 ) ;
#7600 = CIRCLE ( 'NONE', #14737, 0.3000000000000016542 ) ;
#7601 = EDGE_CURVE ( 'NONE', #627, #8987, #14836, .T. ) ;
#7602 = ORIENTED_EDGE ( 'NONE', *, *, #4591, .F. ) ;
#7603 = LINE ( 'NONE', #14397, #12054 ) ;
#7604 = VECTOR ( 'NONE', #3108, 1000.000000000000000 ) ;
#7605 = EDGE_CURVE ( 'NONE', #9043, #440, #4130, .T. ) ;
#7606 = DIRECTION ( 'NONE',  ( -0.000000000000000000, -1.000000000000000000, -0.000000000000000000 ) ) ;
#7607 = FACE_OUTER_BOUND ( 'NONE', #16707, .T. ) ;
#7608 = EDGE_CURVE ( 'NONE', #17937, #16679, #7008, .T. ) ;
#7609 = DIRECTION ( 'NONE',  ( 0.000000000000000000, 0.000000000000000000, -1.000000000000000000 ) ) ;
#7610 = CARTESIAN_POINT ( 'NONE',  ( -29.37573593128808369, -68.87573593128806237, -5.214931150217776400E-15 ) ) ;
#7611 = FACE_OUTER_BOUND ( 'NONE', #7024, .T. ) ;
#7612 = ORIENTED_EDGE ( 'NONE', *, *, #3218, .F. ) ;
#7613 = CARTESIAN_POINT ( 'NONE',  ( 3.127054932750481964, 32.61873716947361856, 42.50000000000000711 ) ) ;
#7614 = VECTOR ( 'NONE', #11446, 1000.000000000000000 ) ;
#7615 = CARTESIAN_POINT ( 'NONE',  ( 23.02398829872514341, -5.683640910026986681, 42.50000000000000000 ) ) ;
#7616 = DIRECTION ( 'NONE',  ( 0.000000000000000000, 1.000000000000000000, 0.000000000000000000 ) ) ;
#7617 = DIRECTION ( 'NONE',  ( -1.000000000000000000, 0.000000000000000000, 0.000000000000000000 ) ) ;
#7618 = EDGE_CURVE ( 'NONE', #10680, #15986, #7352, .T. ) ;
#7619 = CARTESIAN_POINT ( 'NONE',  ( 34.39999999999998437, 85.00000000000000000, 4.249524393041314059E-15 ) ) ;
#7620 = EDGE_LOOP ( 'NONE', ( #5742, #9628, #8690, #2431 ) ) ;
#7621 = ORIENTED_EDGE ( 'NONE', *, *, #16147, .F. ) ;
#7622 = LINE ( 'NONE', #9741, #7828 ) ;
#7623 = CONTEXT_DEPENDENT_SHAPE_REPRESENTATION ( #2707, #16792 ) ;
#7624 = ORIENTED_EDGE ( 'NONE', *, *, #12089, .F. ) ;
#7625 = ORIENTED_EDGE ( 'NONE', *, *, #13336, .F. ) ;
#7626 = DIRECTION ( 'NONE',  ( 1.000000000000000000, 0.000000000000000000, 0.000000000000000000 ) ) ;
#7627 = VERTEX_POINT ( 'NONE', #9011 ) ;
#7628 = DIRECTION ( 'NONE',  ( -8.673617379884034239E-17, 0.000000000000000000, 1.000000000000000000 ) ) ;
#7629 = ADVANCED_FACE ( 'NONE', ( #10797 ), #12454, .F. ) ;
#7630 = EDGE_CURVE ( 'NONE', #6698, #15951, #4513, .T. ) ;
#7631 = CARTESIAN_POINT ( 'NONE',  ( 27.37540678000427619, 7.754037881813018962E-15, 42.50000000000000000 ) ) ;
#7632 = CARTESIAN_POINT ( 'NONE',  ( -30.07540678000427548, 0.000000000000000000, 7.500000000000000000 ) ) ;
#7633 = CARTESIAN_POINT ( 'NONE',  ( 9.641460742840918030, -32.93424481021354921, 68.00000000000000000 ) ) ;
#7634 = DIRECTION ( 'NONE',  ( 0.000000000000000000, -1.000000000000000000, 0.000000000000000000 ) ) ;
#7635 = CARTESIAN_POINT ( 'NONE',  ( 6.424398693589429399E-15, 58.69165929845684104, 70.25000000000000000 ) ) ;
#7636 = CARTESIAN_POINT ( 'NONE',  ( -30.79999999999999361, -84.70000000000001705, 0.3000000000000002665 ) ) ;
#7637 = CARTESIAN_POINT ( 'NONE',  ( -4.603906393579157097, 42.46645089659918426, 70.38908280829822672 ) ) ;
#7638 = DIRECTION ( 'NONE',  ( 0.000000000000000000, -0.000000000000000000, 1.000000000000000000 ) ) ;
#7639 = DIRECTION ( 'NONE',  ( -3.052134192567367925E-16, 1.000000000000000000, 0.000000000000000000 ) ) ;
#7640 = STYLED_ITEM ( 'NONE', ( #5191 ), #16315 ) ;
#7641 = CARTESIAN_POINT ( 'NONE',  ( 15.21174975910705918, -51.86873716947361856, 14.00000000000000000 ) ) ;
#7642 = ORIENTED_EDGE ( 'NONE', *, *, #4694, .F. ) ;
#7643 = ORIENTED_EDGE ( 'NONE', *, *, #7214, .T. ) ;
#7644 = DIRECTION ( 'NONE',  ( 1.000000000000000000, 0.000000000000000000, 0.000000000000000000 ) ) ;
#7645 = EDGE_CURVE ( 'NONE', #6172, #22137, #6212, .T. ) ;
#7646 = ORIENTED_EDGE ( 'NONE', *, *, #15828, .F. ) ;
#7647 = ADVANCED_FACE ( 'NONE', ( #16240 ), #11332, .T. ) ;
#7648 = CARTESIAN_POINT ( 'NONE',  ( -1.824728116533986810, 43.31054587065082728, 37.66679706732590915 ) ) ;
#7649 = AXIS2_PLACEMENT_3D ( 'NONE', #7969, #6187, #12745 ) ;
#7650 = CARTESIAN_POINT ( 'NONE',  ( -1.724728116533986721, 43.31054587065082728, 35.70876104995653577 ) ) ;
#7651 = ORIENTED_EDGE ( 'NONE', *, *, #1039, .F. ) ;
#7652 = DIRECTION ( 'NONE',  ( 0.000000000000000000, 0.000000000000000000, 1.000000000000000000 ) ) ;
#7653 = LINE ( 'NONE', #14447, #20793 ) ;
#7654 = CARTESIAN_POINT ( 'NONE',  ( -28.87540678000428329, 6.494748934539265051, 13.24746166461178554 ) ) ;
#7655 = DIRECTION ( 'NONE',  ( 0.000000000000000000, 0.000000000000000000, 1.000000000000000000 ) ) ;
#7656 = CARTESIAN_POINT ( 'NONE',  ( -23.07462249345254435, 2.431574673422040700, 13.33584746657813902 ) ) ;
#7657 = ORIENTED_EDGE ( 'NONE', *, *, #13340, .T. ) ;
#7658 = DIRECTION ( 'NONE',  ( 0.000000000000000000, 0.000000000000000000, 1.000000000000000000 ) ) ;
#7659 = DIRECTION ( 'NONE',  ( -0.000000000000000000, 1.000000000000000000, -0.000000000000000000 ) ) ;
#7660 = CARTESIAN_POINT ( 'NONE',  ( -32.20000000000001705, -71.00000000000001421, 3.500000000000000000 ) ) ;
#7661 = ORIENTED_EDGE ( 'NONE', *, *, #9309, .T. ) ;
#7662 = ORIENTED_EDGE ( 'NONE', *, *, #21972, .F. ) ;
#7663 = ORIENTED_EDGE ( 'NONE', *, *, #10504, .F. ) ;
#7664 = CARTESIAN_POINT ( 'NONE',  ( 25.37540678000427263, -63.74634676501045050, 7.799999999999999822 ) ) ;
#7666 = EDGE_CURVE ( 'NONE', #2722, #21585, #9495, .T. ) ;
#7665 = LINE ( 'NONE', #4518, #15318 ) ;
#7667 = ORIENTED_EDGE ( 'NONE', *, *, #8477, .F. ) ;
#7668 = EDGE_CURVE ( 'NONE', #16560, #7135, #5949, .T. ) ;
#7669 = DIRECTION ( 'NONE',  ( 0.000000000000000000, -0.000000000000000000, -1.000000000000000000 ) ) ;
#7670 = ORIENTED_EDGE ( 'NONE', *, *, #14368, .T. ) ;
#7671 = CARTESIAN_POINT ( 'NONE',  ( -1.724728116533986721, 43.31054587065082728, 47.75876104995653293 ) ) ;
#7672 = CYLINDRICAL_SURFACE ( 'NONE', #20962, 0.2999999999999947153 ) ;
#7673 = DIRECTION ( 'NONE',  ( -1.000000000000000000, 0.000000000000000000, -0.000000000000000000 ) ) ;
#7674 = CARTESIAN_POINT ( 'NONE',  ( -14.96174975910705207, 50.19799549595485644, 68.50000000000000000 ) ) ;
#7675 = DIRECTION ( 'NONE',  ( -1.000000000000000000, 0.000000000000000000, 0.000000000000000000 ) ) ;
#7676 = DIRECTION ( 'NONE',  ( 0.000000000000000000, 0.000000000000000000, -1.000000000000000000 ) ) ;
#7677 = EDGE_LOOP ( 'NONE', ( #5000, #20905, #4444, #4797 ) ) ;
#7678 = DIRECTION ( 'NONE',  ( 0.000000000000000000, 0.000000000000000000, 1.000000000000000000 ) ) ;
#7679 = CARTESIAN_POINT ( 'NONE',  ( -22.16013893094044462, 45.60883947780118319, 13.50000000000000000 ) ) ;
#7680 = CARTESIAN_POINT ( 'NONE',  ( -14.97529860451076189, 51.91950568661982857, 13.84831215707030339 ) ) ;
#7681 = CARTESIAN_POINT ( 'NONE',  ( 23.32398829872514057, 5.683640910026983128, 13.79999999999999893 ) ) ;
#7682 = EDGE_LOOP ( 'NONE', ( #18474, #13262, #5966, #20809 ) ) ;
#7683 = EDGE_CURVE ( 'NONE', #13748, #17214, #9441, .T. ) ;
#7684 = AXIS2_PLACEMENT_3D ( 'NONE', #7971, #18461, #22063 ) ;
#7685 = CIRCLE ( 'NONE', #12647, 0.2999999999999999334 ) ;
#7686 = VERTEX_POINT ( 'NONE', #17826 ) ;
#7687 = DIRECTION ( 'NONE',  ( 0.000000000000000000, 0.000000000000000000, 1.000000000000000000 ) ) ;
#7688 = DIRECTION ( 'NONE',  ( -0.000000000000000000, 0.000000000000000000, 1.000000000000000000 ) ) ;
#7689 = ORIENTED_EDGE ( 'NONE', *, *, #11853, .T. ) ;
#7690 = ORIENTED_EDGE ( 'NONE', *, *, #9055, .F. ) ;
#7691 = DIRECTION ( 'NONE',  ( 0.000000000000000000, 0.000000000000000000, -1.000000000000000000 ) ) ;
#7692 = CARTESIAN_POINT ( 'NONE',  ( 14.96174975910705918, 41.81054587065082728, 13.75000000000000000 ) ) ;
#7693 = EDGE_CURVE ( 'NONE', #818, #7934, #17341, .T. ) ;
#7694 = EDGE_CURVE ( 'NONE', #22083, #9336, #19146, .T. ) ;
#7695 = CARTESIAN_POINT ( 'NONE',  ( 8.641460742840918030, 33.93424481021354921, 68.50000000000000000 ) ) ;
#7696 = EDGE_LOOP ( 'NONE', ( #1852, #5592, #13065, #6248 ) ) ;
#7697 = ORIENTED_EDGE ( 'NONE', *, *, #16364, .F. ) ;
#7698 = DIRECTION ( 'NONE',  ( 0.000000000000000000, 0.000000000000000000, 1.000000000000000000 ) ) ;
#7699 = AXIS2_PLACEMENT_3D ( 'NONE', #3870, #15814, #158 ) ;
#7700 = ORIENTED_EDGE ( 'NONE', *, *, #3725, .T. ) ;
#7701 = DIRECTION ( 'NONE',  ( 1.000000000000000000, 0.000000000000000000, 0.000000000000000000 ) ) ;
#7702 = DIRECTION ( 'NONE',  ( 0.000000000000000000, -0.000000000000000000, -1.000000000000000000 ) ) ;
#7703 = CARTESIAN_POINT ( 'NONE',  ( 29.17540678000427690, 6.499884319688664647, 7.500000000000000000 ) ) ;
#7704 = CARTESIAN_POINT ( 'NONE',  ( 23.02398829872513986, -2.157133568460768647, 13.19999999999999929 ) ) ;
#7705 = EDGE_CURVE ( 'NONE', #21689, #12623, #924, .T. ) ;
#7706 = DIRECTION ( 'NONE',  ( 2.107255972849994642E-16, -0.000000000000000000, 1.000000000000000000 ) ) ;
#7707 = ORIENTED_EDGE ( 'NONE', *, *, #1796, .F. ) ;
#7708 =( BOUNDED_CURVE ( )  B_SPLINE_CURVE ( 3, ( #4336, #18312, #2986, #19890 ),
 .UNSPECIFIED., .F., .T. ) 
 B_SPLINE_CURVE_WITH_KNOTS ( ( 4, 4 ),
 ( 1.570796326794896558, 3.141592653589793116 ),
 .UNSPECIFIED. ) 
 CURVE ( )  GEOMETRIC_REPRESENTATION_ITEM ( )  RATIONAL_B_SPLINE_CURVE ( ( 1.000000000000000000, 0.8047378541243649375, 0.8047378541243649375, 1.000000000000000000 ) ) 
 REPRESENTATION_ITEM ( '' )  );
#7709 = DIRECTION ( 'NONE',  ( 0.000000000000000000, 0.000000000000000000, -1.000000000000000000 ) ) ;
#7710 = LINE ( 'NONE', #14514, #676 ) ;
#7711 = CYLINDRICAL_SURFACE ( 'NONE', #11872, 0.5000000000000004441 ) ;
#7712 = VECTOR ( 'NONE', #14213, 1000.000000000000000 ) ;
#7713 = VECTOR ( 'NONE', #13367, 1000.000000000000000 ) ;
#7714 = AXIS2_PLACEMENT_3D ( 'NONE', #726, #14047, #13142 ) ;
#7715 = CYLINDRICAL_SURFACE ( 'NONE', #15671, 1.000000000000000888 ) ;
#7716 = EDGE_CURVE ( 'NONE', #20875, #16466, #12894, .T. ) ;
#7717 = EDGE_CURVE ( 'NONE', #6925, #299, #19866, .T. ) ;
#7718 = LINE ( 'NONE', #11067, #17408 ) ;
#7719 = ORIENTED_EDGE ( 'NONE', *, *, #15415, .F. ) ;
#7720 = EDGE_CURVE ( 'NONE', #12463, #20684, #1046, .T. ) ;
#7721 = ORIENTED_EDGE ( 'NONE', *, *, #9291, .F. ) ;
#7722 = ORIENTED_EDGE ( 'NONE', *, *, #9678, .F. ) ;
#7723 = CARTESIAN_POINT ( 'NONE',  ( -25.37540678000427263, 63.74634676501045050, 7.799999999999999822 ) ) ;
#7724 =( REPRESENTATION_RELATIONSHIP ('NONE','NONE', #561, #12850 ) REPRESENTATION_RELATIONSHIP_WITH_TRANSFORMATION ( #4138 )SHAPE_REPRESENTATION_RELATIONSHIP( ) );
#7725 = ORIENTED_EDGE ( 'NONE', *, *, #6404, .T. ) ;
#7726 = ORIENTED_EDGE ( 'NONE', *, *, #2106, .T. ) ;
#7727 = AXIS2_PLACEMENT_3D ( 'NONE', #19471, #6183, #16447 ) ;
#7728 = EDGE_CURVE ( 'NONE', #4820, #6037, #9332, .T. ) ;
#7729 = AXIS2_PLACEMENT_3D ( 'NONE', #16913, #11233, #18055 ) ;
#7730 = VERTEX_POINT ( 'NONE', #7896 ) ;
#7731 = DIRECTION ( 'NONE',  ( 0.000000000000000000, 1.000000000000000000, 0.000000000000000000 ) ) ;
#7732 = AXIS2_PLACEMENT_3D ( 'NONE', #14423, #2682, #6405 ) ;
#7733 = AXIS2_PLACEMENT_3D ( 'NONE', #8338, #18623, #15479 ) ;
#7734 = CARTESIAN_POINT ( 'NONE',  ( -14.96174975910705207, 41.81054587065082728, 13.79999999999999893 ) ) ;
#7735 = DIRECTION ( 'NONE',  ( -8.673617379884034239E-17, -0.000000000000000000, 1.000000000000000000 ) ) ;
#7736 = EDGE_CURVE ( 'NONE', #14744, #21160, #18437, .T. ) ;
#7737 = CYLINDRICAL_SURFACE ( 'NONE', #564, 0.04999999999999991257 ) ;
#7738 = DIRECTION ( 'NONE',  ( -0.000000000000000000, -0.000000000000000000, -1.000000000000000000 ) ) ;
#7739 = CARTESIAN_POINT ( 'NONE',  ( 32.20000000000001705, -71.00000000000001421, 1.800000000000000044 ) ) ;
#7740 = DIRECTION ( 'NONE',  ( 0.000000000000000000, 0.000000000000000000, -1.000000000000000000 ) ) ;
#7741 = DIRECTION ( 'NONE',  ( 0.000000000000000000, 1.000000000000000000, 0.000000000000000000 ) ) ;
#7742 = FACE_OUTER_BOUND ( 'NONE', #19058, .T. ) ;
#7743 = VECTOR ( 'NONE', #17849, 1000.000000000000000 ) ;
#7744 = CARTESIAN_POINT ( 'NONE',  ( 29.20000000000002061, 50.00000000000000000, 0.000000000000000000 ) ) ;
#7745 = AXIS2_PLACEMENT_3D ( 'NONE', #6736, #8065, #19937 ) ;
#7746 = EDGE_CURVE ( 'NONE', #10522, #9296, #816, .T. ) ;
#7747 = ORIENTED_EDGE ( 'NONE', *, *, #8118, .F. ) ;
#7748 = LINE ( 'NONE', #18018, #8105 ) ;
#7749 = ADVANCED_FACE ( 'NONE', ( #5991 ), #12783, .T. ) ;
#7750 = CARTESIAN_POINT ( 'NONE',  ( -17.95292532278785913, -50.11873716947361856, 13.49999999999999822 ) ) ;
#7751 = ORIENTED_EDGE ( 'NONE', *, *, #8838, .T. ) ;
#7752 = ORIENTED_EDGE ( 'NONE', *, *, #9281, .T. ) ;
#7753 = DIRECTION ( 'NONE',  ( 0.000000000000000000, 0.000000000000000000, 1.000000000000000000 ) ) ;
#7754 = ADVANCED_FACE ( 'NONE', ( #13988 ), #22018, .T. ) ;
#7755 = LINE ( 'NONE', #14556, #20283 ) ;
#7756 = ORIENTED_EDGE ( 'NONE', *, *, #4590, .F. ) ;
#7757 = VECTOR ( 'NONE', #3301, 1000.000000000000000 ) ;
#7758 = CIRCLE ( 'NONE', #9540, 0.5000000000000004441 ) ;
#7759 = AXIS2_PLACEMENT_3D ( 'NONE', #9, #11752, #15106 ) ;
#7760 = VECTOR ( 'NONE', #12834, 1000.000000000000000 ) ;
#7761 = EDGE_CURVE ( 'NONE', #20854, #13945, #19269, .T. ) ;
#7762 = CARTESIAN_POINT ( 'NONE',  ( -24.00488095381848197, 42.46645089659918426, 13.74999999999999822 ) ) ;
#7763 = LINE ( 'NONE', #2710, #920 ) ;
#7764 = AXIS2_PLACEMENT_3D ( 'NONE', #12134, #18753, #7017 ) ;
#7765 = ORIENTED_EDGE ( 'NONE', *, *, #62, .T. ) ;
#7766 = CARTESIAN_POINT ( 'NONE',  ( -8.641460742840918030, 32.93424481021354921, 42.50000000000000000 ) ) ;
#7767 = EDGE_CURVE ( 'NONE', #19811, #11511, #5405, .T. ) ;
#7768 = DIRECTION ( 'NONE',  ( 0.000000000000000000, -0.000000000000000000, 1.000000000000000000 ) ) ;
#7769 = CARTESIAN_POINT ( 'NONE',  ( 14.96174975910705740, 51.76873716947361004, 13.50000000000000000 ) ) ;
#7770 = LINE ( 'NONE', #5985, #1480 ) ;
#7771 = CARTESIAN_POINT ( 'NONE',  ( -21.92816239687475743, 42.46645089659918426, 13.50000000000000000 ) ) ;
#7772 = ORIENTED_EDGE ( 'NONE', *, *, #19369, .F. ) ;
#7773 = DIRECTION ( 'NONE',  ( 0.000000000000000000, 1.000000000000000000, 0.000000000000000000 ) ) ;
#7774 = CARTESIAN_POINT ( 'NONE',  ( 15.21174975910705918, 51.86873716947361856, 14.00000000000000000 ) ) ;
#7775 = AXIS2_PLACEMENT_3D ( 'NONE', #15995, #10534, #451 ) ;
#7776 = ORIENTED_EDGE ( 'NONE', *, *, #12619, .F. ) ;
#7777 = VECTOR ( 'NONE', #6733, 1000.000000000000000 ) ;
#7778 = AXIS2_PLACEMENT_3D ( 'NONE', #16438, #11943, #15519 ) ;
#7779 = ORIENTED_EDGE ( 'NONE', *, *, #16341, .T. ) ;
#7780 = ORIENTED_EDGE ( 'NONE', *, *, #10755, .T. ) ;
#7781 = LINE ( 'NONE', #13241, #15620 ) ;
#7782 = EDGE_CURVE ( 'NONE', #2691, #20345, #1269, .T. ) ;
#7783 = DIRECTION ( 'NONE',  ( 0.000000000000000000, -1.000000000000000000, 0.000000000000000000 ) ) ;
#7784 = ORIENTED_EDGE ( 'NONE', *, *, #10675, .F. ) ;
#7785 = VECTOR ( 'NONE', #8767, 1000.000000000000000 ) ;
#7786 = FACE_OUTER_BOUND ( 'NONE', #1854, .T. ) ;
#7787 = VECTOR ( 'NONE', #12666, 1000.000000000000000 ) ;
#7788 = VECTOR ( 'NONE', #11150, 1000.000000000000000 ) ;
#7789 = ORIENTED_EDGE ( 'NONE', *, *, #4358, .T. ) ;
#7790 = CARTESIAN_POINT ( 'NONE',  ( 14.66174975910705847, -42.11054587065083155, 13.50000000000000000 ) ) ;
#7791 = CARTESIAN_POINT ( 'NONE',  ( 15.21174975910707161, -51.86873716947361856, 68.00000000000000000 ) ) ;
#7792 = LINE ( 'NONE', #20098, #8877 ) ;
#7793 = LINE ( 'NONE', #13560, #20236 ) ;
#7794 = CIRCLE ( 'NONE', #20292, 0.2500000000000002220 ) ;
#7795 = VECTOR ( 'NONE', #6226, 1000.000000000000000 ) ;
#7796 = AXIS2_PLACEMENT_3D ( 'NONE', #11485, #9600, #19781 ) ;
#7797 = DIRECTION ( 'NONE',  ( 1.000000000000000000, -1.094601647044990554E-16, 0.000000000000000000 ) ) ;
#7798 = PLANE ( 'NONE',  #13759 ) ;
#7799 = EDGE_LOOP ( 'NONE', ( #13379, #20676, #1130, #10150 ) ) ;
#7800 = DIRECTION ( 'NONE',  ( 0.000000000000000000, 0.000000000000000000, 1.000000000000000000 ) ) ;
#7801 = CYLINDRICAL_SURFACE ( 'NONE', #2471, 0.2999999999999999334 ) ;
#7802 = ADVANCED_FACE ( 'NONE', ( #2244 ), #8865, .F. ) ;
#7803 = B_SPLINE_CURVE_WITH_KNOTS ( 'NONE', 3,
 ( #65, #1618, #4995, #6579 ),
 .UNSPECIFIED., .F., .F.,
 ( 4, 4 ),
 ( 0.005071647684206891972, 0.007900577432593609145 ),
 .UNSPECIFIED. ) ;
#7804 = ADVANCED_FACE ( 'NONE', ( #677 ), #18056, .T. ) ;
#7805 = AXIS2_PLACEMENT_3D ( 'NONE', #10513, #20916, #9054 ) ;
#7806 = DIRECTION ( 'NONE',  ( -0.000000000000000000, -0.000000000000000000, -1.000000000000000000 ) ) ;
#7807 = LINE ( 'NONE', #21571, #11829 ) ;
#7808 = EDGE_LOOP ( 'NONE', ( #17180, #7993, #19921, #6713 ) ) ;
#7809 = EDGE_CURVE ( 'NONE', #4893, #17752, #16257, .T. ) ;
#7810 = DIRECTION ( 'NONE',  ( 0.000000000000000000, 0.000000000000000000, -1.000000000000000000 ) ) ;
#7811 = AXIS2_PLACEMENT_3D ( 'NONE', #16119, #7644, #11309 ) ;
#7812 = DIRECTION ( 'NONE',  ( 0.000000000000000000, 0.000000000000000000, 1.000000000000000000 ) ) ;
#7813 = AXIS2_PLACEMENT_3D ( 'NONE', #7470, #19527, #17625 ) ;
#7814 = EDGE_LOOP ( 'NONE', ( #12060, #12826, #14439, #3997 ) ) ;
#7815 = FACE_OUTER_BOUND ( 'NONE', #431, .T. ) ;
#7816 = DIRECTION ( 'NONE',  ( 0.000000000000000000, 1.000000000000000000, 0.000000000000000000 ) ) ;
#7817 = ORIENTED_EDGE ( 'NONE', *, *, #9994, .T. ) ;
#7818 = EDGE_LOOP ( 'NONE', ( #3688, #14483, #1492, #6940 ) ) ;
#7819 = CYLINDRICAL_SURFACE ( 'NONE', #608, 0.2999999999999999889 ) ;
#7820 = CARTESIAN_POINT ( 'NONE',  ( 26.56227312273159313, 9.958410664601840878, 42.50000000000000000 ) ) ;
#7821 = CARTESIAN_POINT ( 'NONE',  ( -1.724728116533986721, 42.36054587065083155, 27.75876104995654003 ) ) ;
#7822 = AXIS2_PLACEMENT_3D ( 'NONE', #9125, #14149, #15933 ) ;
#7823 = VECTOR ( 'NONE', #1582, 1000.000000000000000 ) ;
#7824 = VERTEX_POINT ( 'NONE', #17471 ) ;
#7825 = AXIS2_PLACEMENT_3D ( 'NONE', #5574, #12357, #19213 ) ;
#7826 = EDGE_LOOP ( 'NONE', ( #210, #4020, #7162, #11633 ) ) ;
#7827 = CYLINDRICAL_SURFACE ( 'NONE', #13955, 0.6000000000000033085 ) ;
#7828 = VECTOR ( 'NONE', #16441, 1000.000000000000000 ) ;
#7829 = TOROIDAL_SURFACE ( 'NONE', #4252, 2.767785046117003489, 0.2500000000000000000 ) ;
#7830 = CARTESIAN_POINT ( 'NONE',  ( -23.32398829872514057, -2.157133568460768647, 13.50000000000000000 ) ) ;
#7831 = CARTESIAN_POINT ( 'NONE',  ( 32.20000000000001705, 0.000000000000000000, 1.500000000000000000 ) ) ;
#7832 = CARTESIAN_POINT ( 'NONE',  ( -20.53081511603577525, 86.49759185912193971, 13.75000000000000000 ) ) ;
#7833 = DIRECTION ( 'NONE',  ( 0.000000000000000000, -0.000000000000000000, 1.000000000000000000 ) ) ;
#7834 = DIRECTION ( 'NONE',  ( 0.000000000000000000, 0.000000000000000000, 1.000000000000000000 ) ) ;
#7835 = EDGE_CURVE ( 'NONE', #412, #3965, #20220, .T. ) ;
#7836 = CARTESIAN_POINT ( 'NONE',  ( -21.92816239687475743, 42.46645089659918426, 13.50000000000000000 ) ) ;
#7837 = CYLINDRICAL_SURFACE ( 'NONE', #15648, 0.2500000000000002220 ) ;
#7838 = ORIENTED_EDGE ( 'NONE', *, *, #308, .F. ) ;
#7839 = AXIS2_PLACEMENT_3D ( 'NONE', #5365, #1534, #1969 ) ;
#7840 = CARTESIAN_POINT ( 'NONE',  ( -9.641460742840918030, -32.61873716947361856, 109.6002446535588319 ) ) ;
#7841 = CARTESIAN_POINT ( 'NONE',  ( 1.774728116533979883, 42.36054587065083155, 41.66679706732590915 ) ) ;
#7842 = AXIS2_PLACEMENT_3D ( 'NONE', #14118, #154, #12008 ) ;
#7843 = DIRECTION ( 'NONE',  ( 0.000000000000000000, 0.000000000000000000, 1.000000000000000000 ) ) ;
#7844 = CIRCLE ( 'NONE', #3913, 0.5000000000000004441 ) ;
#7845 = CARTESIAN_POINT ( 'NONE',  ( -30.79999999999999361, -84.70000000000001705, 2.571758278209446887E-16 ) ) ;
#7846 = DIRECTION ( 'NONE',  ( 0.000000000000000000, 0.000000000000000000, -1.000000000000000000 ) ) ;
#7847 = ORIENTED_EDGE ( 'NONE', *, *, #5661, .F. ) ;
#7848 = ORIENTED_EDGE ( 'NONE', *, *, #14869, .F. ) ;
#7849 = DIRECTION ( 'NONE',  ( 1.000000000000000000, 0.000000000000000000, 0.000000000000000000 ) ) ;
#7850 = VERTEX_POINT ( 'NONE', #20729 ) ;
#7851 = DIRECTION ( 'NONE',  ( 1.000000000000000000, 0.000000000000000000, 0.000000000000000000 ) ) ;
#7852 = ORIENTED_EDGE ( 'NONE', *, *, #11893, .F. ) ;
#7853 = DIRECTION ( 'NONE',  ( 1.224646799147353207E-16, 0.000000000000000000, 1.000000000000000000 ) ) ;
#7854 = AXIS2_PLACEMENT_3D ( 'NONE', #10415, #11956, #8391 ) ;
#7855 = VERTEX_POINT ( 'NONE', #7525 ) ;
#7856 = EDGE_CURVE ( 'NONE', #9562, #12188, #12526, .T. ) ;
#7857 = DIRECTION ( 'NONE',  ( -0.000000000000000000, -1.000000000000000000, -0.000000000000000000 ) ) ;
#7858 = LINE ( 'NONE', #11186, #13055 ) ;
#7859 = CARTESIAN_POINT ( 'NONE',  ( 30.19999999999999574, 70.29999999999999716, 1.500000000000003997 ) ) ;
#7860 = EDGE_CURVE ( 'NONE', #15183, #7877, #10649, .T. ) ;
#7861 = FACE_OUTER_BOUND ( 'NONE', #9298, .T. ) ;
#7862 = CARTESIAN_POINT ( 'NONE',  ( 28.87540678000427619, 0.000000000000000000, 13.50000000000000000 ) ) ;
#7863 = DIRECTION ( 'NONE',  ( 1.094601647044983281E-16, 1.000000000000000000, 0.000000000000000000 ) ) ;
#7864 = CARTESIAN_POINT ( 'NONE',  ( 23.32398829872514412, -5.683640910026986681, 13.50000000000000000 ) ) ;
#7865 = CARTESIAN_POINT ( 'NONE',  ( 30.67540678000428045, 63.74634676501045050, 3.799999999999999822 ) ) ;
#7866 = AXIS2_PLACEMENT_3D ( 'NONE', #19182, #19075, #12123 ) ;
#7867 = ORIENTED_EDGE ( 'NONE', *, *, #6269, .T. ) ;
#7868 = CARTESIAN_POINT ( 'NONE',  ( -29.69597781366221412, 27.99124249474150972, 68.50000000000000000 ) ) ;
#7869 = AXIS2_PLACEMENT_3D ( 'NONE', #5017, #1530, #14964 ) ;
#7870 = AXIS2_PLACEMENT_3D ( 'NONE', #7340, #10699, #10806 ) ;
#7871 = DIRECTION ( 'NONE',  ( -1.734723475976806848E-16, 0.000000000000000000, 1.000000000000000000 ) ) ;
#7872 = ORIENTED_EDGE ( 'NONE', *, *, #637, .F. ) ;
#7873 = ORIENTED_EDGE ( 'NONE', *, *, #16006, .F. ) ;
#7874 = LINE ( 'NONE', #9659, #19578 ) ;
#7875 = DIRECTION ( 'NONE',  ( 1.000000000000000000, 0.000000000000000000, 0.000000000000000000 ) ) ;
#7876 = EDGE_CURVE ( 'NONE', #9461, #4063, #2137, .T. ) ;
#7877 = VERTEX_POINT ( 'NONE', #21068 ) ;
#7878 = EDGE_LOOP ( 'NONE', ( #7289, #11021, #12337, #4994 ) ) ;
#7879 = ORIENTED_EDGE ( 'NONE', *, *, #1039, .T. ) ;
#7880 = ADVANCED_FACE ( 'NONE', ( #4046 ), #19375, .T. ) ;
#7881 = CIRCLE ( 'NONE', #20387, 0.2999999999999999334 ) ;
#7882 = EDGE_CURVE ( 'NONE', #21191, #8611, #2354, .T. ) ;
#7883 = CIRCLE ( 'NONE', #4287, 0.2500000000000002220 ) ;
#7884 = CARTESIAN_POINT ( 'NONE',  ( 15.05577974591271051, -52.39333374568191459, 13.50000000000000000 ) ) ;
#7885 = VECTOR ( 'NONE', #4506, 1000.000000000000000 ) ;
#7886 = EDGE_CURVE ( 'NONE', #22033, #341, #4493, .T. ) ;
#7887 = CARTESIAN_POINT ( 'NONE',  ( -14.96174975910705207, 32.10873716947361345, 13.05380965755523448 ) ) ;
#7888 = VERTEX_POINT ( 'NONE', #2474 ) ;
#7889 = DIRECTION ( 'NONE',  ( -0.000000000000000000, -0.000000000000000000, 1.000000000000000000 ) ) ;
#7890 = ADVANCED_FACE ( 'NONE', ( #15776 ), #227, .F. ) ;
#7891 = CARTESIAN_POINT ( 'NONE',  ( 3.627054932750481964, -32.61873716947361856, 7.321391277662001151 ) ) ;
#7892 = DIRECTION ( 'NONE',  ( 0.000000000000000000, 1.000000000000000000, -0.000000000000000000 ) ) ;
#7893 = DIRECTION ( 'NONE',  ( 0.000000000000000000, -0.000000000000000000, -1.000000000000000000 ) ) ;
#7894 = ORIENTED_EDGE ( 'NONE', *, *, #16324, .T. ) ;
#7895 = DIRECTION ( 'NONE',  ( -2.546383084002652634E-16, 0.000000000000000000, -1.000000000000000000 ) ) ;
#7896 = CARTESIAN_POINT ( 'NONE',  ( 1.774728116533979438, 42.31054587065082728, 43.80876104995653719 ) ) ;
#7897 = EDGE_LOOP ( 'NONE', ( #18233, #18166, #14445, #17620 ) ) ;
#7898 = ORIENTED_EDGE ( 'NONE', *, *, #6958, .T. ) ;
#7899 = VERTEX_POINT ( 'NONE', #7296 ) ;
#7900 = CARTESIAN_POINT ( 'NONE',  ( 14.97552947837228032, 51.92046840034491595, 13.84856038353110463 ) ) ;
#7901 = AXIS2_PLACEMENT_3D ( 'NONE', #16005, #7638, #19385 ) ;
#7902 = DIRECTION ( 'NONE',  ( 1.000000000000000000, 0.000000000000000000, 0.000000000000000000 ) ) ;
#7903 = EDGE_CURVE ( 'NONE', #21314, #11510, #6654, .T. ) ;
#7904 = ORIENTED_EDGE ( 'NONE', *, *, #21020, .T. ) ;
#7905 = ORIENTED_EDGE ( 'NONE', *, *, #8769, .F. ) ;
#7906 = CARTESIAN_POINT ( 'NONE',  ( -1.724728116533986721, 42.31054587065082728, 43.75876104995654003 ) ) ;
#7907 = CARTESIAN_POINT ( 'NONE',  ( -28.57540678000427548, -63.74634676501045050, 13.50000000000000000 ) ) ;
#7908 = EDGE_CURVE ( 'NONE', #15670, #5317, #11990, .T. ) ;
#7909 = CARTESIAN_POINT ( 'NONE',  ( -3.127054932750481964, -32.11873716947361856, 42.50000000000000711 ) ) ;
#7910 = DIRECTION ( 'NONE',  ( 1.000000000000000000, 0.000000000000000000, 0.000000000000000000 ) ) ;
#7911 = EDGE_LOOP ( 'NONE', ( #9322, #1438, #17055, #17038 ) ) ;
#7912 = CARTESIAN_POINT ( 'NONE',  ( -9.641460742840918030, -33.43424481021354921, 68.00000000000000000 ) ) ;
#7913 = EDGE_CURVE ( 'NONE', #6717, #10573, #14853, .T. ) ;
#7914 = CARTESIAN_POINT ( 'NONE',  ( -29.69597781366221412, 26.24124249474150972, 70.50000000000000000 ) ) ;
#7915 = VECTOR ( 'NONE', #6591, 1000.000000000000000 ) ;
#7916 = CARTESIAN_POINT ( 'NONE',  ( -14.96174975910705207, 51.76873716947361714, 13.79999999999999716 ) ) ;
#7917 = PLANE ( 'NONE',  #19750 ) ;
#7918 = ORIENTED_EDGE ( 'NONE', *, *, #7860, .F. ) ;
#7919 = FACE_OUTER_BOUND ( 'NONE', #15344, .T. ) ;
#7920 = DIRECTION ( 'NONE',  ( -1.000000000000000000, 0.000000000000000000, 0.000000000000000000 ) ) ;
#7921 = ORIENTED_EDGE ( 'NONE', *, *, #8563, .T. ) ;
#7922 = DIRECTION ( 'NONE',  ( 0.000000000000000000, 0.000000000000000000, -1.000000000000000000 ) ) ;
#7923 = DIRECTION ( 'NONE',  ( 1.000000000000000000, 0.000000000000000000, 0.000000000000000000 ) ) ;
#7924 = ORIENTED_EDGE ( 'NONE', *, *, #6370, .F. ) ;
#7925 = VERTEX_POINT ( 'NONE', #9409 ) ;
#7926 = EDGE_LOOP ( 'NONE', ( #21914, #10474, #11199 ) ) ;
#7927 = DIRECTION ( 'NONE',  ( 0.000000000000000000, 0.000000000000000000, 1.000000000000000000 ) ) ;
#7928 = CARTESIAN_POINT ( 'NONE',  ( 17.95292532278785913, 34.11873716947361856, 68.00000000000000000 ) ) ;
#7929 = DIRECTION ( 'NONE',  ( -1.000000000000000000, 0.000000000000000000, 0.000000000000000000 ) ) ;
#7930 = VECTOR ( 'NONE', #19301, 1000.000000000000000 ) ;
#7931 = ORIENTED_EDGE ( 'NONE', *, *, #17818, .T. ) ;
#7932 = ADVANCED_FACE ( 'NONE', ( #11412 ), #8428, .T. ) ;
#7933 = EDGE_CURVE ( 'NONE', #4677, #10096, #11275, .T. ) ;
#7934 = VERTEX_POINT ( 'NONE', #11292 ) ;
#7935 = CARTESIAN_POINT ( 'NONE',  ( -29.50000000000002132, 0.000000000000000000, 1.500000000000000000 ) ) ;
#7936 = DIRECTION ( 'NONE',  ( -1.000000000000000000, 0.000000000000000000, -0.000000000000000000 ) ) ;
#7937 = CARTESIAN_POINT ( 'NONE',  ( 17.45292532278785913, 34.11873716947361856, 68.00000000000000000 ) ) ;
#7938 = CIRCLE ( 'NONE', #10783, 0.5000000000000000000 ) ;
#7939 = DIRECTION ( 'NONE',  ( 0.000000000000000000, 1.000000000000000000, 0.000000000000000000 ) ) ;
#7940 = FACE_OUTER_BOUND ( 'NONE', #3290, .T. ) ;
#7941 = DIRECTION ( 'NONE',  ( 0.000000000000000000, 0.000000000000000000, 1.000000000000000000 ) ) ;
#7942 = VERTEX_POINT ( 'NONE', #18122 ) ;
#7943 = EDGE_CURVE ( 'NONE', #12460, #225, #14124, .T. ) ;
#7944 = CYLINDRICAL_SURFACE ( 'NONE', #14935, 0.2999999999999999334 ) ;
#7945 = VECTOR ( 'NONE', #5773, 1000.000000000000000 ) ;
#7946 = VECTOR ( 'NONE', #22055, 1000.000000000000000 ) ;
#7947 = CARTESIAN_POINT ( 'NONE',  ( 1.774728116533973665, 43.26054587065083012, 4.000000000000000000 ) ) ;
#7948 = DIRECTION ( 'NONE',  ( 2.107255972849994642E-16, -0.000000000000000000, 1.000000000000000000 ) ) ;
#7949 = EDGE_LOOP ( 'NONE', ( #13485, #4752, #14196, #7726, #1159, #20503, #8721, #8921 ) ) ;
#7950 = DIRECTION ( 'NONE',  ( 2.107255972849994642E-16, -0.000000000000000000, 1.000000000000000000 ) ) ;
#7951 = DIRECTION ( 'NONE',  ( 1.000000000000000000, -0.000000000000000000, -0.000000000000000000 ) ) ;
#7952 = ORIENTED_EDGE ( 'NONE', *, *, #16173, .T. ) ;
#7953 = DIRECTION ( 'NONE',  ( 1.000000000000000000, 0.000000000000000000, 0.000000000000000000 ) ) ;
#7954 = ORIENTED_EDGE ( 'NONE', *, *, #6996, .T. ) ;
#7955 = ORIENTED_EDGE ( 'NONE', *, *, #21703, .F. ) ;
#7956 = CARTESIAN_POINT ( 'NONE',  ( -1.836970198721029934E-16, -71.70000000000001705, 3.200000000000000178 ) ) ;
#7957 = ADVANCED_FACE ( 'NONE', ( #21510 ), #14868, .F. ) ;
#7958 = VECTOR ( 'NONE', #15856, 1000.000000000000000 ) ;
#7959 = ORIENTED_EDGE ( 'NONE', *, *, #6924, .F. ) ;
#7960 = EDGE_CURVE ( 'NONE', #15046, #12241, #12856, .T. ) ;
#7961 = DIRECTION ( 'NONE',  ( 0.000000000000000000, 0.000000000000000000, 1.000000000000000000 ) ) ;
#7962 = CARTESIAN_POINT ( 'NONE',  ( -8.638906393579159015, 40.01645089659919563, 70.88527860057354246 ) ) ;
#7963 = DIRECTION ( 'NONE',  ( 0.000000000000000000, 0.000000000000000000, 1.000000000000000000 ) ) ;
#7964 = DIRECTION ( 'NONE',  ( -0.000000000000000000, -1.000000000000000000, 0.000000000000000000 ) ) ;
#7965 = CARTESIAN_POINT ( 'NONE',  ( -29.13662752439705272, 0.000000000000000000, 3.500000000000000000 ) ) ;
#7966 = CARTESIAN_POINT ( 'NONE',  ( 14.96174975910707161, 32.10873716947361345, 68.25000000000000000 ) ) ;
#7967 = FACE_OUTER_BOUND ( 'NONE', #21175, .T. ) ;
#7968 = CIRCLE ( 'NONE', #7254, 0.3000000000000016542 ) ;
#7969 = CARTESIAN_POINT ( 'NONE',  ( 1.724728116533979616, 43.31054587065082728, 35.80876104995653009 ) ) ;
#7970 = FACE_OUTER_BOUND ( 'NONE', #1079, .T. ) ;
#7972 = EDGE_CURVE ( 'NONE', #16984, #22089, #206, .T. ) ;
#7971 = CARTESIAN_POINT ( 'NONE',  ( -29.13662752439705272, 0.000000000000000000, 3.799999999999999822 ) ) ;
#7973 = ORIENTED_EDGE ( 'NONE', *, *, #18683, .T. ) ;
#7974 = CARTESIAN_POINT ( 'NONE',  ( 9.641460742840918030, 32.61873716947361856, 68.00000000000000000 ) ) ;
#7975 = CARTESIAN_POINT ( 'NONE',  ( 33.79999999999999005, -84.70000000000001705, 78.20000000000000284 ) ) ;
#7976 = ORIENTED_EDGE ( 'NONE', *, *, #18558, .F. ) ;
#7977 = VERTEX_POINT ( 'NONE', #7734 ) ;
#7978 = DIRECTION ( 'NONE',  ( -1.000000000000000000, 0.000000000000000000, 0.000000000000000000 ) ) ;
#7979 = ADVANCED_FACE ( 'NONE', ( #5951 ), #4849, .T. ) ;
#7980 = DIRECTION ( 'NONE',  ( 1.000000000000000000, 0.000000000000000000, 0.000000000000000000 ) ) ;
#7981 = EDGE_CURVE ( 'NONE', #1455, #17364, #4475, .T. ) ;
#7982 = ORIENTED_EDGE ( 'NONE', *, *, #21540, .T. ) ;
#7983 = ORIENTED_EDGE ( 'NONE', *, *, #4745, .T. ) ;
#7984 = EDGE_LOOP ( 'NONE', ( #3088, #15728, #7400, #15236 ) ) ;
#7985 = DIRECTION ( 'NONE',  ( -1.000000000000000000, 0.000000000000000000, 0.000000000000000000 ) ) ;
#7986 = CARTESIAN_POINT ( 'NONE',  ( 26.63662752439704917, 3.061616997868386099E-16, 1.500000000000001332 ) ) ;
#7987 = VERTEX_POINT ( 'NONE', #14533 ) ;
#7988 = FILL_AREA_STYLE ('',( #6315 ) ) ;
#7989 = EDGE_CURVE ( 'NONE', #2179, #12457, #12348, .T. ) ;
#7990 = CARTESIAN_POINT ( 'NONE',  ( -3.127054932750481964, 32.11873716947361856, 42.50000000000000711 ) ) ;
#7991 = LINE ( 'NONE', #4746, #20076 ) ;
#7992 = CARTESIAN_POINT ( 'NONE',  ( -29.13662752439705272, 0.000000000000000000, -18.50000000000000000 ) ) ;
#7993 = ORIENTED_EDGE ( 'NONE', *, *, #406, .F. ) ;
#7994 = DIRECTION ( 'NONE',  ( 0.000000000000000000, 0.000000000000000000, 1.000000000000000000 ) ) ;
#7995 = EDGE_LOOP ( 'NONE', ( #19437, #2398, #17684, #16980 ) ) ;
#7996 = ORIENTED_EDGE ( 'NONE', *, *, #757, .T. ) ;
#7997 = ORIENTED_EDGE ( 'NONE', *, *, #21419, .T. ) ;
#7998 = CARTESIAN_POINT ( 'NONE',  ( 23.04273156199908357, -2.261510999192740901, 13.19999999999999929 ) ) ;
#7999 = DIRECTION ( 'NONE',  ( 0.000000000000000000, 0.000000000000000000, 1.000000000000000000 ) ) ;
#8000 = EDGE_CURVE ( 'NONE', #9706, #19294, #22040, .T. ) ;
#8001 = ORIENTED_EDGE ( 'NONE', *, *, #7389, .T. ) ;
#8002 = EDGE_CURVE ( 'NONE', #2490, #3783, #20045, .T. ) ;
#8003 = CARTESIAN_POINT ( 'NONE',  ( 0.000000000000000000, 43.31054587065082728, 20.00000000000000000 ) ) ;
#8004 = ORIENTED_EDGE ( 'NONE', *, *, #6493, .F. ) ;
#8005 = MECHANICAL_DESIGN_GEOMETRIC_PRESENTATION_REPRESENTATION (  '', ( #17264 ), #19416 ) ;
#8006 = CARTESIAN_POINT ( 'NONE',  ( -32.50000000000002132, 71.00000000000001421, 1.800000000000000044 ) ) ;
#8007 = CARTESIAN_POINT ( 'NONE',  ( 34.69999999999998863, -85.00000000000000000, 0.6000000000000033085 ) ) ;
#8008 = LINE ( 'NONE', #4763, #17428 ) ;
#8009 = DIRECTION ( 'NONE',  ( 1.000000000000000000, 0.000000000000000000, 0.000000000000000000 ) ) ;
#8010 = VERTEX_POINT ( 'NONE', #19812 ) ;
#8011 = DIRECTION ( 'NONE',  ( -1.000000000000000000, 0.000000000000000000, 0.000000000000000000 ) ) ;
#8012 = CARTESIAN_POINT ( 'NONE',  ( 30.79999999999999716, -84.70000000000001705, 1.200000000000004174 ) ) ;
#8013 = ADVANCED_FACE ( 'NONE', ( #16445 ), #19162, .T. ) ;
#8014 = TOROIDAL_SURFACE ( 'NONE', #12983, 2.076718556943726313, 0.2500000000000000000 ) ;
#8015 = CARTESIAN_POINT ( 'NONE',  ( 29.69597781366221767, 58.69165929845684104, 68.75000000000000000 ) ) ;
#8016 = DIRECTION ( 'NONE',  ( 0.000000000000000000, 1.000000000000000000, 0.000000000000000000 ) ) ;
#8017 = ORIENTED_EDGE ( 'NONE', *, *, #11750, .F. ) ;
#8018 = CARTESIAN_POINT ( 'NONE',  ( -14.71174975910705029, 51.86873716947361856, 14.00000000000000000 ) ) ;
#8019 = DIRECTION ( 'NONE',  ( 0.000000000000000000, 0.000000000000000000, -1.000000000000000000 ) ) ;
#8020 = APPLICATION_CONTEXT ( 'automotive_design' ) ;
#8021 = VERTEX_POINT ( 'NONE', #18009 ) ;
#8022 = LINE ( 'NONE', #1283, #21297 ) ;
#8023 = CARTESIAN_POINT ( 'NONE',  ( 15.21174975910707161, 52.11873716947361856, 68.00000000000000000 ) ) ;
#8024 = CIRCLE ( 'NONE', #3212, 0.2999999999999999889 ) ;
#8025 = ORIENTED_EDGE ( 'NONE', *, *, #7422, .F. ) ;
#8026 = AXIS2_PLACEMENT_3D ( 'NONE', #20763, #12449, #20866 ) ;
#8027 = ORIENTED_EDGE ( 'NONE', *, *, #6982, .F. ) ;
#8028 = ORIENTED_EDGE ( 'NONE', *, *, #149, .T. ) ;
#8029 = DIRECTION ( 'NONE',  ( -6.123233995736764803E-17, 0.000000000000000000, 1.000000000000000000 ) ) ;
#8030 = CARTESIAN_POINT ( 'NONE',  ( -29.69597781366221412, 27.99124249474150972, 70.50000000000000000 ) ) ;
#8031 = EDGE_CURVE ( 'NONE', #1986, #3697, #9514, .T. ) ;
#8032 = CARTESIAN_POINT ( 'NONE',  ( 34.99999999999999289, 84.70000000000001705, 0.6000000000000033085 ) ) ;
#8033 = EDGE_CURVE ( 'NONE', #16460, #21635, #3806, .T. ) ;
#8034 = ORIENTED_EDGE ( 'NONE', *, *, #907, .F. ) ;
#8035 = EDGE_CURVE ( 'NONE', #8963, #1590, #1447, .T. ) ;
#8036 = ORIENTED_EDGE ( 'NONE', *, *, #13104, .F. ) ;
#8037 = CARTESIAN_POINT ( 'NONE',  ( 33.19999999999999574, -85.00000000000000000, 78.50000000000000000 ) ) ;
#8038 = CARTESIAN_POINT ( 'NONE',  ( 23.02398829872513986, 2.157133568460765538, 7.500000000000000000 ) ) ;
#8039 = DIRECTION ( 'NONE',  ( 1.000000000000000000, 0.000000000000000000, 0.000000000000000000 ) ) ;
#8040 = FACE_OUTER_BOUND ( 'NONE', #220, .T. ) ;
#8041 = CARTESIAN_POINT ( 'NONE',  ( -1.724728116533986721, 43.26054587065083012, 49.66679706732590915 ) ) ;
#8042 = AXIS2_PLACEMENT_3D ( 'NONE', #1706, #7096, #5310 ) ;
#8043 = DIRECTION ( 'NONE',  ( -0.000000000000000000, 0.000000000000000000, 1.000000000000000000 ) ) ;
#8044 = CARTESIAN_POINT ( 'NONE',  ( -23.02398829872514341, -5.683640910026986681, 42.50000000000000000 ) ) ;
#8045 = PRODUCT_DEFINITION_SHAPE ( 'NONE', 'NONE',  #7141 ) ;
#8046 = DIRECTION ( 'NONE',  ( -1.000000000000000000, 0.000000000000000000, 0.000000000000000000 ) ) ;
#8047 = VERTEX_POINT ( 'NONE', #1551 ) ;
#8048 = DIRECTION ( 'NONE',  ( -1.000000000000000000, 0.000000000000000000, 0.000000000000000000 ) ) ;
#8049 = EDGE_CURVE ( 'NONE', #11393, #20783, #9966, .T. ) ;
#8050 = LINE ( 'NONE', #17883, #14363 ) ;
#8051 = ORIENTED_EDGE ( 'NONE', *, *, #11793, .F. ) ;
#8052 = CARTESIAN_POINT ( 'NONE',  ( -26.56227312273159313, 9.958410664601840878, 42.50000000000000000 ) ) ;
#8053 = DIRECTION ( 'NONE',  ( 0.000000000000000000, -1.000000000000000000, 0.000000000000000000 ) ) ;
#8054 = ORIENTED_EDGE ( 'NONE', *, *, #5946, .T. ) ;
#8055 = AXIS2_PLACEMENT_3D ( 'NONE', #5478, #15334, #7363 ) ;
#8056 = ORIENTED_EDGE ( 'NONE', *, *, #12900, .T. ) ;
#8057 = AXIS2_PLACEMENT_3D ( 'NONE', #1536, #14972, #5251 ) ;
#8058 = PLANE ( 'NONE',  #11668 ) ;
#8059 = ADVANCED_FACE ( 'NONE', ( #18684 ), #13861, .T. ) ;
#8060 = VERTEX_POINT ( 'NONE', #1792 ) ;
#8061 = DIRECTION ( 'NONE',  ( 0.000000000000000000, 0.000000000000000000, -1.000000000000000000 ) ) ;
#8062 = CARTESIAN_POINT ( 'NONE',  ( -9.178906393579158163, 42.46645089659918426, 70.38908280829822672 ) ) ;
#8063 = VECTOR ( 'NONE', #21373, 1000.000000000000000 ) ;
#8064 = CARTESIAN_POINT ( 'NONE',  ( -9.641460742840918030, 32.61873716947361856, 68.00000000000000000 ) ) ;
#8065 = DIRECTION ( 'NONE',  ( -1.000000000000000000, -0.000000000000000000, -0.000000000000000000 ) ) ;
#8066 = CARTESIAN_POINT ( 'NONE',  ( 23.02398829872513986, 3.395978615688218571, 13.79999998357615532 ) ) ;
#8067 = CARTESIAN_POINT ( 'NONE',  ( -9.718906393579157310, 41.43704565779017202, 70.88527860057354246 ) ) ;
#8068 = AXIS2_PLACEMENT_3D ( 'NONE', #18404, #3420, #3083 ) ;
#8069 = AXIS2_PLACEMENT_3D ( 'NONE', #15702, #2057, #19184 ) ;
#8070 = AXIS2_PLACEMENT_3D ( 'NONE', #9906, #9695, #2742 ) ;
#8071 = CARTESIAN_POINT ( 'NONE',  ( 1.724728116533979616, 42.36054587065083155, 35.80876104995653009 ) ) ;
#8072 = EDGE_CURVE ( 'NONE', #17208, #18524, #2795, .T. ) ;
#8073 = DIRECTION ( 'NONE',  ( 0.000000000000000000, 0.000000000000000000, -1.000000000000000000 ) ) ;
#8074 = ADVANCED_FACE ( 'NONE', ( #13309 ), #18885, .F. ) ;
#8075 = DIRECTION ( 'NONE',  ( -0.000000000000000000, -1.000000000000000000, -0.000000000000000000 ) ) ;
#8076 = ORIENTED_EDGE ( 'NONE', *, *, #20400, .F. ) ;
#8077 = CARTESIAN_POINT ( 'NONE',  ( -1.724728116533986721, 43.26054587065083012, 41.76679706732590347 ) ) ;
#8078 = ORIENTED_EDGE ( 'NONE', *, *, #1491, .T. ) ;
#8079 = DIRECTION ( 'NONE',  ( 0.000000000000000000, 1.000000000000000000, -0.000000000000000000 ) ) ;
#8081 = DIRECTION ( 'NONE',  ( 1.000000000000000000, 0.000000000000000000, 0.000000000000000000 ) ) ;
#8080 = AXIS2_PLACEMENT_3D ( 'NONE', #20903, #12158, #12370 ) ;
#8082 = VERTEX_POINT ( 'NONE', #6850 ) ;
#8083 = CIRCLE ( 'NONE', #16276, 0.2500000000000002220 ) ;
#8084 = VERTEX_POINT ( 'NONE', #15436 ) ;
#8085 = LINE ( 'NONE', #14890, #13151 ) ;
#8086 = SHAPE_REPRESENTATION_RELATIONSHIP ( 'NONE' , 'NONE' ,  #12850, #13111 ) ;
#8087 = VERTEX_POINT ( 'NONE', #3354 ) ;
#8088 = CARTESIAN_POINT ( 'NONE',  ( -4.127054932750482408, -33.43424481021354921, 68.00000000000000000 ) ) ;
#8089 = AXIS2_PLACEMENT_3D ( 'NONE', #9224, #6105, #21316 ) ;
#8090 = VECTOR ( 'NONE', #18968, 1000.000000000000000 ) ;
#8091 = ORIENTED_EDGE ( 'NONE', *, *, #1493, .F. ) ;
#8092 = ORIENTED_EDGE ( 'NONE', *, *, #6834, .T. ) ;
#8093 = EDGE_CURVE ( 'NONE', #15871, #13456, #5672, .T. ) ;
#8094 = ORIENTED_EDGE ( 'NONE', *, *, #12972, .F. ) ;
#8095 = CARTESIAN_POINT ( 'NONE',  ( 14.71479891986436606, -52.07369784111803312, 13.50000000000000000 ) ) ;
#8096 = AXIS2_PLACEMENT_3D ( 'NONE', #2247, #7194, #20842 ) ;
#8097 = AXIS2_PLACEMENT_3D ( 'NONE', #19334, #14058, #5370 ) ;
#8098 = DIRECTION ( 'NONE',  ( 0.000000000000000000, 0.000000000000000000, 1.000000000000000000 ) ) ;
#8099 = ORIENTED_EDGE ( 'NONE', *, *, #7933, .F. ) ;
#8100 = CARTESIAN_POINT ( 'NONE',  ( 0.000000000000000000, 51.61873716947361856, 68.00000000000000000 ) ) ;
#8101 = EDGE_CURVE ( 'NONE', #20941, #7686, #1668, .T. ) ;
#8102 = CARTESIAN_POINT ( 'NONE',  ( 30.67540678000428045, 63.74634676501045050, 3.500000000000000000 ) ) ;
#8103 = DIRECTION ( 'NONE',  ( 0.000000000000000000, -0.000000000000000000, 1.000000000000000000 ) ) ;
#8104 = CARTESIAN_POINT ( 'NONE',  ( -29.09616827897941249, 6.500357068115323322, 7.499999999998635758 ) ) ;
#8105 = VECTOR ( 'NONE', #10982, 1000.000000000000000 ) ;
#8106 = DIRECTION ( 'NONE',  ( -1.000000000000000000, 0.000000000000000000, 0.000000000000000000 ) ) ;
#8107 = EDGE_LOOP ( 'NONE', ( #19396, #13816, #14032, #16011 ) ) ;
#8108 = ORIENTED_EDGE ( 'NONE', *, *, #11877, .T. ) ;
#8109 = ORIENTED_EDGE ( 'NONE', *, *, #8719, .F. ) ;
#8110 = CARTESIAN_POINT ( 'NONE',  ( 0.000000000000000000, -51.61873716947361856, 68.00000000000000000 ) ) ;
#8111 = DIRECTION ( 'NONE',  ( 1.000000000000000000, 0.000000000000000000, 0.000000000000000000 ) ) ;
#8112 = ORIENTED_EDGE ( 'NONE', *, *, #12062, .T. ) ;
#8113 = AXIS2_PLACEMENT_3D ( 'NONE', #13009, #940, #13356 ) ;
#8114 = CIRCLE ( 'NONE', #21344, 2.076718556943725424 ) ;
#8115 = VECTOR ( 'NONE', #4333, 1000.000000000000000 ) ;
#8116 = DIRECTION ( 'NONE',  ( 0.2309407893632117181, -0.9729678061520313781, 0.000000000000000000 ) ) ;
#8117 = VECTOR ( 'NONE', #8364, 1000.000000000000000 ) ;
#8118 = EDGE_CURVE ( 'NONE', #10999, #13328, #9225, .T. ) ;
#8119 = VERTEX_POINT ( 'NONE', #109 ) ;
#8120 = DIRECTION ( 'NONE',  ( -0.9729678061520339316, -0.2309407893632008379, 1.418549243141864450E-14 ) ) ;
#8121 = CIRCLE ( 'NONE', #21352, 0.2999999999999999889 ) ;
#8122 = DIRECTION ( 'NONE',  ( -1.000000000000000000, 0.000000000000000000, 0.000000000000000000 ) ) ;
#8123 = DIRECTION ( 'NONE',  ( 1.000000000000000000, 0.000000000000000000, 0.000000000000000000 ) ) ;
#8124 = FACE_OUTER_BOUND ( 'NONE', #20855, .T. ) ;
#8125 = VERTEX_POINT ( 'NONE', #6955 ) ;
#8126 = CARTESIAN_POINT ( 'NONE',  ( -14.71174975910705029, 51.61873716947361856, 68.00000000000000000 ) ) ;
#8127 = EDGE_CURVE ( 'NONE', #8176, #8431, #19575, .T. ) ;
#8128 = AXIS2_PLACEMENT_3D ( 'NONE', #14443, #1031, #18030 ) ;
#8129 = EDGE_CURVE ( 'NONE', #13945, #11867, #12073, .T. ) ;
#8130 = CARTESIAN_POINT ( 'NONE',  ( 29.37540678000427619, -6.000000000000000000, 7.200000000000000178 ) ) ;
#8131 = DIRECTION ( 'NONE',  ( 0.000000000000000000, 0.000000000000000000, -1.000000000000000000 ) ) ;
#8132 = ORIENTED_EDGE ( 'NONE', *, *, #18542, .F. ) ;
#8133 = CIRCLE ( 'NONE', #21345, 4.351418481279133665 ) ;
#8134 = LINE ( 'NONE', #21898, #10914 ) ;
#8135 = VERTEX_POINT ( 'NONE', #15200 ) ;
#8136 = FACE_OUTER_BOUND ( 'NONE', #3291, .T. ) ;
#8137 = AXIS2_PLACEMENT_3D ( 'NONE', #2854, #11224, #12899 ) ;
#8138 = CARTESIAN_POINT ( 'NONE',  ( 29.13662752439705272, 0.000000000000000000, 7.200000000000000178 ) ) ;
#8139 = ORIENTED_EDGE ( 'NONE', *, *, #17435, .T. ) ;
#8140 = ORIENTED_EDGE ( 'NONE', *, *, #3228, .T. ) ;
#8141 = VECTOR ( 'NONE', #10345, 1000.000000000000000 ) ;
#8142 = ORIENTED_EDGE ( 'NONE', *, *, #11521, .F. ) ;
#8143 = DIRECTION ( 'NONE',  ( -1.000000000000000000, 3.009265538104883829E-28, -4.336808689941893885E-15 ) ) ;
#8144 = CARTESIAN_POINT ( 'NONE',  ( -29.50000000000002132, 69.00000000000000000, 1.500000000000000000 ) ) ;
#8145 = VERTEX_POINT ( 'NONE', #11616 ) ;
#8146 = EDGE_CURVE ( 'NONE', #11890, #19753, #15098, .T. ) ;
#8147 = ORIENTED_EDGE ( 'NONE', *, *, #8536, .F. ) ;
#8148 = CIRCLE ( 'NONE', #1334, 0.2500000000000002220 ) ;
#8149 = CARTESIAN_POINT ( 'NONE',  ( 29.20000000000002061, 68.70000000000001705, 0.000000000000000000 ) ) ;
#8150 = CIRCLE ( 'NONE', #14192, 0.5000000000000004441 ) ;
#8151 = AXIS2_PLACEMENT_3D ( 'NONE', #8959, #21054, #5732 ) ;
#8152 = CARTESIAN_POINT ( 'NONE',  ( -1.774728116533986766, 43.31054587065082728, 53.66679706732590915 ) ) ;
#8153 = DIRECTION ( 'NONE',  ( -0.000000000000000000, -0.000000000000000000, 1.000000000000000000 ) ) ;
#8154 = DIRECTION ( 'NONE',  ( 1.000000000000000000, 0.000000000000000000, 0.000000000000000000 ) ) ;
#8155 = DIRECTION ( 'NONE',  ( 1.000000000000000000, 0.000000000000000000, 0.000000000000000000 ) ) ;
#8156 = CIRCLE ( 'NONE', #975, 0.5000000000000004441 ) ;
#8157 = CARTESIAN_POINT ( 'NONE',  ( -6.728906393579160650, 43.00645089659919762, 70.88527860057354246 ) ) ;
#8158 = AXIS2_PLACEMENT_3D ( 'NONE', #1752, #20449, #11581 ) ;
#8159 = CARTESIAN_POINT ( 'NONE',  ( 30.37540678000427619, 0.000000000000000000, 7.200000000000000178 ) ) ;
#8160 = EDGE_CURVE ( 'NONE', #5001, #4119, #21380, .T. ) ;
#8161 = ADVANCED_FACE ( 'NONE', ( #6735 ), #1331, .T. ) ;
#8162 = DIRECTION ( 'NONE',  ( 1.000000000000000000, -0.000000000000000000, 0.000000000000000000 ) ) ;
#8163 = CARTESIAN_POINT ( 'NONE',  ( -9.641460742840918030, 32.61873716947361856, 68.00000000000000000 ) ) ;
#8164 = ORIENTED_EDGE ( 'NONE', *, *, #7705, .T. ) ;
#8165 = CYLINDRICAL_SURFACE ( 'NONE', #15535, 0.2999999999999999334 ) ;
#8166 = EDGE_CURVE ( 'NONE', #22136, #7338, #16708, .T. ) ;
#8167 = CARTESIAN_POINT ( 'NONE',  ( 0.000000000000000000, 67.24634676501045760, 7.799999999999999822 ) ) ;
#8168 = DIRECTION ( 'NONE',  ( -1.000000000000000000, 0.000000000000000000, -8.673617379883930701E-17 ) ) ;
#8169 = AXIS2_PLACEMENT_3D ( 'NONE', #5567, #2297, #12245 ) ;
#8170 = TOROIDAL_SURFACE ( 'NONE', #2787, 2.767785046117003489, 0.2500000000000000000 ) ;
#8171 = VERTEX_POINT ( 'NONE', #21838 ) ;
#8172 = CARTESIAN_POINT ( 'NONE',  ( 15.21174975910707161, 42.31054587065082728, 68.50000000000000000 ) ) ;
#8173 = DIRECTION ( 'NONE',  ( 1.000000000000000000, 3.543406725251269872E-15, -1.224646799147353207E-16 ) ) ;
#8174 = ORIENTED_EDGE ( 'NONE', *, *, #473, .T. ) ;
#8175 = VECTOR ( 'NONE', #14844, 1000.000000000000000 ) ;
#8176 = VERTEX_POINT ( 'NONE', #18571 ) ;
#8177 = CIRCLE ( 'NONE', #14217, 0.2999999999999999334 ) ;
#8178 = CARTESIAN_POINT ( 'NONE',  ( 25.37540678000427263, 67.24634676501045760, 13.19999999999999929 ) ) ;
#8179 = AXIS2_PLACEMENT_3D ( 'NONE', #19319, #2299, #20891 ) ;
#8180 = ADVANCED_FACE ( 'NONE', ( #22056 ), #15635, .T. ) ;
#8181 = VERTEX_POINT ( 'NONE', #10082 ) ;
#8182 = CYLINDRICAL_SURFACE ( 'NONE', #3137, 0.2999999999999999334 ) ;
#8183 = FACE_OUTER_BOUND ( 'NONE', #4236, .T. ) ;
#8184 = AXIS2_PLACEMENT_3D ( 'NONE', #12932, #16690, #10107 ) ;
#8185 = CARTESIAN_POINT ( 'NONE',  ( 33.19999999999999574, 84.70000000000001705, 78.20000000000000284 ) ) ;
#8186 = CARTESIAN_POINT ( 'NONE',  ( 29.13662752439705272, 0.000000000000000000, 0.3000000000000016542 ) ) ;
#8187 = DIRECTION ( 'NONE',  ( 0.000000000000000000, 0.000000000000000000, -1.000000000000000000 ) ) ;
#8188 = AXIS2_PLACEMENT_3D ( 'NONE', #20687, #20792, #17198 ) ;
#8189 = ADVANCED_FACE ( 'NONE', ( #5495 ), #3801, .T. ) ;
#8190 = DIRECTION ( 'NONE',  ( 1.000000000000000000, 0.000000000000000000, 0.000000000000000000 ) ) ;
#8191 = LINE ( 'NONE', #15101, #14327 ) ;
#8192 = EDGE_CURVE ( 'NONE', #19749, #712, #14299, .T. ) ;
#8193 = DIRECTION ( 'NONE',  ( 1.000000000000000000, 0.000000000000000000, 0.000000000000000000 ) ) ;
#8194 = CARTESIAN_POINT ( 'NONE',  ( 15.21174975910707161, 52.11873716947361856, 68.00000000000000000 ) ) ;
#8195 = DIRECTION ( 'NONE',  ( 0.000000000000000000, 0.000000000000000000, 1.000000000000000000 ) ) ;
#8196 = EDGE_LOOP ( 'NONE', ( #19542, #18337, #21643, #8554 ) ) ;
#8197 = FACE_OUTER_BOUND ( 'NONE', #15423, .T. ) ;
#8198 = VERTEX_POINT ( 'NONE', #12504 ) ;
#8199 = CARTESIAN_POINT ( 'NONE',  ( -29.50000000000002132, -2.473451120191013430, -150.0833101980363722 ) ) ;
#8200 = DIRECTION ( 'NONE',  ( 1.000000000000000000, 0.000000000000000000, 0.000000000000000000 ) ) ;
#8201 = EDGE_LOOP ( 'NONE', ( #20417, #18208, #13522, #14404 ) ) ;
#8202 = CARTESIAN_POINT ( 'NONE',  ( -11.62890639357915923, 41.92645089659917801, 70.88527860057354246 ) ) ;
#8203 = CIRCLE ( 'NONE', #6054, 0.2999999999999999334 ) ;
#8204 = FILL_AREA_STYLE ('',( #1356 ) ) ;
#8205 = ORIENTED_EDGE ( 'NONE', *, *, #11769, .T. ) ;
#8206 = AXIS2_PLACEMENT_3D ( 'NONE', #4577, #984, #12950 ) ;
#8207 = EDGE_CURVE ( 'NONE', #18926, #11864, #17797, .T. ) ;
#8208 = ORIENTED_EDGE ( 'NONE', *, *, #1580, .F. ) ;
#8209 = EDGE_CURVE ( 'NONE', #8021, #1401, #7088, .T. ) ;
#8210 = ORIENTED_EDGE ( 'NONE', *, *, #18754, .F. ) ;
#8211 = CARTESIAN_POINT ( 'NONE',  ( 14.98281217233416562, -51.83338592095527275, 13.50000000000000000 ) ) ;
#8212 = DIRECTION ( 'NONE',  ( -0.000000000000000000, -1.000000000000000000, -0.000000000000000000 ) ) ;
#8213 = ORIENTED_EDGE ( 'NONE', *, *, #2256, .F. ) ;
#8214 = DIRECTION ( 'NONE',  ( -0.2309407893632007824, 0.9729678061520339316, 0.000000000000000000 ) ) ;
#8215 = AXIS2_PLACEMENT_3D ( 'NONE', #21250, #17982, #18092 ) ;
#8216 = VECTOR ( 'NONE', #6024, 1000.000000000000000 ) ;
#8217 = CARTESIAN_POINT ( 'NONE',  ( -23.26560317237337117, 3.297643262788010787, 13.49417356369015231 ) ) ;
#8218 = CARTESIAN_POINT ( 'NONE',  ( -17.95292532278785913, -34.11873716947361856, 42.50000000000000711 ) ) ;
#8219 = DIRECTION ( 'NONE',  ( -1.000000000000000000, 0.000000000000000000, 0.000000000000000000 ) ) ;
#8220 = DIRECTION ( 'NONE',  ( -0.000000000000000000, -0.000000000000000000, -1.000000000000000000 ) ) ;
#8221 = ORIENTED_EDGE ( 'NONE', *, *, #12398, .F. ) ;
#8222 = ORIENTED_EDGE ( 'NONE', *, *, #22026, .T. ) ;
#8223 = ORIENTED_EDGE ( 'NONE', *, *, #7856, .F. ) ;
#8224 = FACE_OUTER_BOUND ( 'NONE', #6889, .T. ) ;
#8225 = DIRECTION ( 'NONE',  ( -1.000000000000000000, 0.000000000000000000, -0.000000000000000000 ) ) ;
#8226 = EDGE_LOOP ( 'NONE', ( #11577, #4889, #11133, #12522 ) ) ;
#8227 = DIRECTION ( 'NONE',  ( 0.000000000000000000, -1.000000000000000000, 0.000000000000000000 ) ) ;
#8228 = AXIS2_PLACEMENT_3D ( 'NONE', #15405, #12030, #18879 ) ;
#8229 = CIRCLE ( 'NONE', #18584, 0.5000000000000004441 ) ;
#8230 = ORIENTED_EDGE ( 'NONE', *, *, #386, .F. ) ;
#8231 = CARTESIAN_POINT ( 'NONE',  ( -8.149501154770138811, 41.92645089659918511, 70.88527860057354246 ) ) ;
#8232 = EDGE_CURVE ( 'NONE', #14977, #4119, #8949, .T. ) ;
#8233 = DIRECTION ( 'NONE',  ( 1.000000000000000000, 0.000000000000000000, 0.000000000000000000 ) ) ;
#8234 = DIRECTION ( 'NONE',  ( -0.000000000000000000, 1.000000000000000000, 0.000000000000000000 ) ) ;
#8235 = ORIENTED_EDGE ( 'NONE', *, *, #601, .F. ) ;
#8236 = DIRECTION ( 'NONE',  ( 1.000000000000000000, -0.000000000000000000, -0.000000000000000000 ) ) ;
#8237 = DIRECTION ( 'NONE',  ( 0.000000000000000000, 1.000000000000000000, 0.000000000000000000 ) ) ;
#8238 = DIRECTION ( 'NONE',  ( 0.000000000000000000, 0.000000000000000000, 1.000000000000000000 ) ) ;
#8239 = CARTESIAN_POINT ( 'NONE',  ( -28.87540678000427619, -63.74634676501045050, 7.799999999999999822 ) ) ;
#8240 = ORIENTED_EDGE ( 'NONE', *, *, #19691, .T. ) ;
#8241 = LINE ( 'NONE', #15156, #10223 ) ;
#8242 = CIRCLE ( 'NONE', #21480, 0.05000000000000143219 ) ;
#8243 = VERTEX_POINT ( 'NONE', #203 ) ;
#8244 = AXIS2_PLACEMENT_3D ( 'NONE', #13333, #16918, #10109 ) ;
#8245 = DIRECTION ( 'NONE',  ( 0.000000000000000000, 0.000000000000000000, -1.000000000000000000 ) ) ;
#8246 = LINE ( 'NONE', #4670, #11647 ) ;
#8247 = EDGE_CURVE ( 'NONE', #6694, #6444, #17431, .T. ) ;
#8248 = VERTEX_POINT ( 'NONE', #15751 ) ;
#8249 = ORIENTED_EDGE ( 'NONE', *, *, #4866, .F. ) ;
#8250 = VERTEX_POINT ( 'NONE', #19348 ) ;
#8251 = DIRECTION ( 'NONE',  ( 1.000000000000000000, 0.000000000000000000, 0.000000000000000000 ) ) ;
#8252 = VERTEX_POINT ( 'NONE', #318 ) ;
#8253 = DIRECTION ( 'NONE',  ( 0.000000000000000000, 0.000000000000000000, 1.000000000000000000 ) ) ;
#8254 = EDGE_CURVE ( 'NONE', #4674, #7580, #16355, .T. ) ;
#8255 = ORIENTED_EDGE ( 'NONE', *, *, #5256, .T. ) ;
#8256 = ADVANCED_FACE ( 'NONE', ( #20706 ), #5383, .F. ) ;
#8257 = ORIENTED_EDGE ( 'NONE', *, *, #11258, .F. ) ;
#8258 = CARTESIAN_POINT ( 'NONE',  ( 15.21174975910705918, -52.11873716947361856, 14.00000000000000000 ) ) ;
#8259 = DIRECTION ( 'NONE',  ( 0.000000000000000000, -0.000000000000000000, -1.000000000000000000 ) ) ;
#8260 = CYLINDRICAL_SURFACE ( 'NONE', #8498, 0.2999999999999999334 ) ;
#8261 = VECTOR ( 'NONE', #3357, 1000.000000000000000 ) ;
#8262 = CARTESIAN_POINT ( 'NONE',  ( 34.39999999999998437, 84.70000000000001705, 4.249524393041314059E-15 ) ) ;
#8263 = DIRECTION ( 'NONE',  ( 0.000000000000000000, 1.000000000000000000, 0.000000000000000000 ) ) ;
#8264 = CARTESIAN_POINT ( 'NONE',  ( -23.02398829872513986, 5.683640910026983128, 13.79999999999999893 ) ) ;
#8265 = VERTEX_POINT ( 'NONE', #3590 ) ;
#8266 = LINE ( 'NONE', #8159, #17110 ) ;
#8267 = CARTESIAN_POINT ( 'NONE',  ( -17.92752199202934094, -38.74634676501045760, 13.79999999999999893 ) ) ;
#8268 = FACE_OUTER_BOUND ( 'NONE', #13875, .T. ) ;
#8269 = B_SPLINE_CURVE_WITH_KNOTS ( 'NONE', 3,
 ( #15682, #20954, #3841, #8983, #19161, #5642, #458, #20849 ),
 .UNSPECIFIED., .F., .F.,
 ( 4, 2, 2, 4 ),
 ( 0.000000000000000000, 0.0002421094859592866821, 0.0003631642289389202518, 0.0004842189719185537944 ),
 .UNSPECIFIED. ) ;
#8270 = ORIENTED_EDGE ( 'NONE', *, *, #15, .F. ) ;
#8271 = CARTESIAN_POINT ( 'NONE',  ( -31.69597781366221412, 26.24124249474150972, 68.75000000000000000 ) ) ;
#8272 = ADVANCED_FACE ( 'NONE', ( #1891 ), #20817, .T. ) ;
#8273 = VECTOR ( 'NONE', #7658, 1000.000000000000000 ) ;
#8274 = CARTESIAN_POINT ( 'NONE',  ( 27.37540678000427974, -10.94079601157914716, 42.50000000000000000 ) ) ;
#8275 = EDGE_LOOP ( 'NONE', ( #15032, #15363, #1198, #18802 ) ) ;
#8276 = CYLINDRICAL_SURFACE ( 'NONE', #16718, 0.5000000000000004441 ) ;
#8277 = AXIS2_PLACEMENT_3D ( 'NONE', #9451, #21777, #14706 ) ;
#8278 = EDGE_LOOP ( 'NONE', ( #10896, #20061, #19850, #16225 ) ) ;
#8279 = EDGE_LOOP ( 'NONE', ( #14698, #2849, #11373, #968 ) ) ;
#8280 = DIRECTION ( 'NONE',  ( 0.000000000000000000, 0.000000000000000000, 1.000000000000000000 ) ) ;
#8281 = ADVANCED_FACE ( 'NONE', ( #7060 ), #12171, .T. ) ;
#8282 = EDGE_CURVE ( 'NONE', #1986, #8181, #2440, .T. ) ;
#8283 = AXIS2_PLACEMENT_3D ( 'NONE', #21646, #18155, #9435 ) ;
#8284 = ADVANCED_FACE ( 'NONE', ( #3923 ), #22105, .F. ) ;
#8285 = VERTEX_POINT ( 'NONE', #13961 ) ;
#8286 = EDGE_CURVE ( 'NONE', #5550, #2970, #7383, .T. ) ;
#8287 = CARTESIAN_POINT ( 'NONE',  ( -14.71174975910705029, 51.61873716947361856, 13.75000000000000000 ) ) ;
#8288 = ORIENTED_EDGE ( 'NONE', *, *, #15164, .F. ) ;
#8289 = LINE ( 'NONE', #19810, #4190 ) ;
#8290 = AXIS2_PLACEMENT_3D ( 'NONE', #3728, #7309, #12207 ) ;
#8291 = LINE ( 'NONE', #6615, #8775 ) ;
#8292 = CARTESIAN_POINT ( 'NONE',  ( 0.000000000000000000, -68.70000000000001705, 0.000000000000000000 ) ) ;
#8293 = DIRECTION ( 'NONE',  ( 1.000000000000000000, 0.000000000000000000, 0.000000000000000000 ) ) ;
#8294 = FACE_OUTER_BOUND ( 'NONE', #2847, .T. ) ;
#8295 = DIRECTION ( 'NONE',  ( -0.000000000000000000, 1.000000000000000000, -0.000000000000000000 ) ) ;
#8296 = EDGE_CURVE ( 'NONE', #11899, #19336, #1359, .T. ) ;
#8297 = DIRECTION ( 'NONE',  ( 0.000000000000000000, 0.000000000000000000, 1.000000000000000000 ) ) ;
#8298 = CARTESIAN_POINT ( 'NONE',  ( -15.00250675241655429, -51.98442790175712247, 13.86082508289638149 ) ) ;
#8299 = DIRECTION ( 'NONE',  ( 0.000000000000000000, 1.000000000000000000, 0.000000000000000000 ) ) ;
#8300 = AXIS2_PLACEMENT_3D ( 'NONE', #11131, #12581, #14270 ) ;
#8301 = AXIS2_PLACEMENT_3D ( 'NONE', #892, #11191, #20053 ) ;
#8302 = DIRECTION ( 'NONE',  ( -0.000000000000000000, -1.000000000000000000, -0.000000000000000000 ) ) ;
#8303 = VERTEX_POINT ( 'NONE', #9162 ) ;
#8304 = CARTESIAN_POINT ( 'NONE',  ( -34.70000000000001705, 84.70000000000001705, 79.39999999999999147 ) ) ;
#8305 = AXIS2_PLACEMENT_3D ( 'NONE', #6046, #5921, #17652 ) ;
#8306 = ORIENTED_EDGE ( 'NONE', *, *, #14344, .F. ) ;
#8307 = ORIENTED_EDGE ( 'NONE', *, *, #4762, .T. ) ;
#8308 = LINE ( 'NONE', #5060, #10995 ) ;
#8309 = CARTESIAN_POINT ( 'NONE',  ( 0.000000000000000000, 0.000000000000000000, 0.000000000000000000 ) ) ;
#8310 = ORIENTED_EDGE ( 'NONE', *, *, #34, .F. ) ;
#8311 = EDGE_CURVE ( 'NONE', #8671, #17214, #13146, .T. ) ;
#8312 = ADVANCED_FACE ( 'NONE', ( #16424 ), #21701, .T. ) ;
#8313 = EDGE_LOOP ( 'NONE', ( #18006, #3545, #13612, #8288 ) ) ;
#8314 = ORIENTED_EDGE ( 'NONE', *, *, #9612, .F. ) ;
#8315 = AXIS2_PLACEMENT_3D ( 'NONE', #21048, #5608, #17562 ) ;
#8316 = CARTESIAN_POINT ( 'NONE',  ( 1.724728116533979616, 43.26054587065083012, 35.75876104995654003 ) ) ;
#8317 = CARTESIAN_POINT ( 'NONE',  ( -34.40000000000001279, 85.00000000000000000, 79.39999999999999147 ) ) ;
#8318 = AXIS2_PLACEMENT_3D ( 'NONE', #15584, #4876, #11685 ) ;
#8319 = ORIENTED_EDGE ( 'NONE', *, *, #1561, .F. ) ;
#8320 = DIRECTION ( 'NONE',  ( 0.000000000000000000, 1.000000000000000000, 0.000000000000000000 ) ) ;
#8321 = CARTESIAN_POINT ( 'NONE',  ( -23.02398829872513986, 3.418849134688105362, 13.52821124852824397 ) ) ;
#8322 = CARTESIAN_POINT ( 'NONE',  ( -9.718906393579157310, 41.66638367286108746, 68.06527860057354928 ) ) ;
#8323 = DIRECTION ( 'NONE',  ( 0.000000000000000000, 0.000000000000000000, 1.000000000000000000 ) ) ;
#8324 = CIRCLE ( 'NONE', #19390, 1.000000000000000888 ) ;
#8325 = EDGE_CURVE ( 'NONE', #10005, #8815, #21369, .T. ) ;
#8326 = DIRECTION ( 'NONE',  ( 1.000000000000000000, -0.000000000000000000, 0.000000000000000000 ) ) ;
#8327 = ORIENTED_EDGE ( 'NONE', *, *, #11988, .F. ) ;
#8328 = ORIENTED_EDGE ( 'NONE', *, *, #3509, .F. ) ;
#8329 = VERTEX_POINT ( 'NONE', #14630 ) ;
#8330 = DIRECTION ( 'NONE',  ( -0.000000000000000000, -0.000000000000000000, -1.000000000000000000 ) ) ;
#8331 = CARTESIAN_POINT ( 'NONE',  ( -29.50000000000002842, -2.473451120191013874, 0.2503166595423103602 ) ) ;
#8332 = ORIENTED_EDGE ( 'NONE', *, *, #10323, .F. ) ;
#8333 = EDGE_CURVE ( 'NONE', #15347, #15161, #8598, .T. ) ;
#8334 = ORIENTED_EDGE ( 'NONE', *, *, #10937, .F. ) ;
#8335 = DIRECTION ( 'NONE',  ( 1.000000000000000000, -0.000000000000000000, 0.000000000000000000 ) ) ;
#8336 = DIRECTION ( 'NONE',  ( -0.000000000000000000, -0.000000000000000000, 1.000000000000000000 ) ) ;
#8337 = CARTESIAN_POINT ( 'NONE',  ( -23.61959064016851073, 45.26242829375641463, 13.74999999999999822 ) ) ;
#8338 = CARTESIAN_POINT ( 'NONE',  ( -1.724728116533986721, 42.36054587065083155, 51.80876104995653719 ) ) ;
#8339 = VERTEX_POINT ( 'NONE', #19681 ) ;
#8340 = CARTESIAN_POINT ( 'NONE',  ( -1.724728116533986721, 42.31054587065082728, 29.71679706732590631 ) ) ;
#8341 = DIRECTION ( 'NONE',  ( -1.000000000000000000, 0.000000000000000000, 0.000000000000000000 ) ) ;
#8342 = PLANE ( 'NONE',  #7593 ) ;
#8343 = DIRECTION ( 'NONE',  ( -1.000000000000000000, 0.000000000000000000, 0.000000000000000000 ) ) ;
#8344 = SURFACE_STYLE_FILL_AREA ( #18740 ) ;
#8345 = VERTEX_POINT ( 'NONE', #861 ) ;
#8346 = DIRECTION ( 'NONE',  ( 1.000000000000000000, -0.000000000000000000, 0.000000000000000000 ) ) ;
#8347 = EDGE_CURVE ( 'NONE', #8339, #16466, #992, .T. ) ;
#8348 = EDGE_LOOP ( 'NONE', ( #12721, #11125, #17615, #18645 ) ) ;
#8349 = FACE_OUTER_BOUND ( 'NONE', #2366, .T. ) ;
#8350 = LINE ( 'NONE', #15159, #3461 ) ;
#8351 = EDGE_LOOP ( 'NONE', ( #17824, #16339, #6766, #5798 ) ) ;
#8352 = ORIENTED_EDGE ( 'NONE', *, *, #12349, .F. ) ;
#8353 = ORIENTED_EDGE ( 'NONE', *, *, #18893, .T. ) ;
#8354 = DIRECTION ( 'NONE',  ( 0.000000000000000000, 0.000000000000000000, -1.000000000000000000 ) ) ;
#8355 = DIRECTION ( 'NONE',  ( 0.000000000000000000, 1.000000000000000000, 0.000000000000000000 ) ) ;
#8356 = ORIENTED_EDGE ( 'NONE', *, *, #11805, .T. ) ;
#8357 = CARTESIAN_POINT ( 'NONE',  ( 33.19999999999999574, 84.70000000000001705, 1.799999999999996048 ) ) ;
#8358 = EDGE_LOOP ( 'NONE', ( #11540, #22010, #9702, #5368 ) ) ;
#8359 = ORIENTED_EDGE ( 'NONE', *, *, #20735, .F. ) ;
#8360 = CARTESIAN_POINT ( 'NONE',  ( -25.37540678000427263, 67.54634676501045476, 7.799999999999999822 ) ) ;
#8361 = CIRCLE ( 'NONE', #6233, 4.575000000000001066 ) ;
#8362 = ORIENTED_EDGE ( 'NONE', *, *, #4592, .T. ) ;
#8363 = CARTESIAN_POINT ( 'NONE',  ( 0.000000000000000000, 0.000000000000000000, 13.50000000000000000 ) ) ;
#8364 = DIRECTION ( 'NONE',  ( 1.000000000000000000, 0.000000000000000000, -0.000000000000000000 ) ) ;
#8365 = EDGE_CURVE ( 'NONE', #416, #7987, #3871, .T. ) ;
#8366 = DIRECTION ( 'NONE',  ( 1.000000000000000000, 0.000000000000000000, 0.000000000000000000 ) ) ;
#8367 = CARTESIAN_POINT ( 'NONE',  ( -9.178906393579158163, 42.46645089659918426, 67.85468508031152624 ) ) ;
#8368 = CARTESIAN_POINT ( 'NONE',  ( 0.000000000000000000, -67.24634676501045760, 7.799999999999999822 ) ) ;
#8369 = AXIS2_PLACEMENT_3D ( 'NONE', #13421, #11747, #10086 ) ;
#8370 = DIRECTION ( 'NONE',  ( -4.336808689941893885E-15, 0.000000000000000000, 1.000000000000000000 ) ) ;
#8371 = CARTESIAN_POINT ( 'NONE',  ( -9.718906393579157310, 41.42245079618239600, 68.06527860057354928 ) ) ;
#8372 = AXIS2_PLACEMENT_3D ( 'NONE', #18815, #10322, #13751 ) ;
#8373 = ORIENTED_EDGE ( 'NONE', *, *, #7761, .F. ) ;
#8374 = LINE ( 'NONE', #15185, #9479 ) ;
#8375 = AXIS2_PLACEMENT_3D ( 'NONE', #8576, #8452, #20104 ) ;
#8376 = ADVANCED_FACE ( 'NONE', ( #18095 ), #7944, .T. ) ;
#8377 = DIRECTION ( 'NONE',  ( -0.000000000000000000, -0.000000000000000000, 1.000000000000000000 ) ) ;
#8378 = VERTEX_POINT ( 'NONE', #11057 ) ;
#8379 = LINE ( 'NONE', #1777, #14957 ) ;
#8380 = LINE ( 'NONE', #20478, #13858 ) ;
#8381 = VERTEX_POINT ( 'NONE', #2449 ) ;
#8382 = ORIENTED_EDGE ( 'NONE', *, *, #3776, .F. ) ;
#8383 = FACE_OUTER_BOUND ( 'NONE', #7396, .T. ) ;
#8384 = ORIENTED_EDGE ( 'NONE', *, *, #15664, .T. ) ;
#8385 = EDGE_CURVE ( 'NONE', #9771, #4245, #19449, .T. ) ;
#8386 = CARTESIAN_POINT ( 'NONE',  ( -14.71174975910705029, 50.19799549595485644, 68.25000000000000000 ) ) ;
#8387 = CARTESIAN_POINT ( 'NONE',  ( -29.33570773061603276, 2.657594995084290979, 0.02220324760240992637 ) ) ;
#8388 = CYLINDRICAL_SURFACE ( 'NONE', #7218, 0.2500000000000002220 ) ;
#8389 = DIRECTION ( 'NONE',  ( 0.000000000000000000, 0.000000000000000000, 1.000000000000000000 ) ) ;
#8390 = DIRECTION ( 'NONE',  ( 0.000000000000000000, -1.000000000000000000, 0.000000000000000000 ) ) ;
#8391 = DIRECTION ( 'NONE',  ( -1.000000000000000000, 0.000000000000000000, 0.000000000000000000 ) ) ;
#8392 = DIRECTION ( 'NONE',  ( -0.000000000000000000, 1.000000000000000000, -0.000000000000000000 ) ) ;
#8393 = ADVANCED_FACE ( 'NONE', ( #1193 ), #6392, .T. ) ;
#8394 = ADVANCED_FACE ( 'NONE', ( #4122 ), #6263, .T. ) ;
#8395 = CARTESIAN_POINT ( 'NONE',  ( 27.37540678000427619, 5.683640910026986681, 13.79999999999999893 ) ) ;
#8396 = EDGE_CURVE ( 'NONE', #21935, #4820, #4249, .T. ) ;
#8397 = CARTESIAN_POINT ( 'NONE',  ( 34.39999999999998437, -84.70000000000001705, 80.00000000000000000 ) ) ;
#8398 = CIRCLE ( 'NONE', #11242, 0.2999999999999999334 ) ;
#8399 = CIRCLE ( 'NONE', #6981, 0.2999999999999999334 ) ;
#8400 = CYLINDRICAL_SURFACE ( 'NONE', #6722, 0.1000000000000028644 ) ;
#8401 = ORIENTED_EDGE ( 'NONE', *, *, #9391, .T. ) ;
#8402 = DIRECTION ( 'NONE',  ( 0.000000000000000000, 0.000000000000000000, 1.000000000000000000 ) ) ;
#8403 = LINE ( 'NONE', #15215, #8521 ) ;
#8404 = ORIENTED_EDGE ( 'NONE', *, *, #35, .T. ) ;
#8405 = VERTEX_POINT ( 'NONE', #16081 ) ;
#8406 = DIRECTION ( 'NONE',  ( -1.000000000000000000, 0.000000000000000000, 0.000000000000000000 ) ) ;
#8407 = ORIENTED_EDGE ( 'NONE', *, *, #6811, .T. ) ;
#8408 = ADVANCED_FACE ( 'NONE', ( #10943 ), #4571, .T. ) ;
#8409 = VERTEX_POINT ( 'NONE', #7704 ) ;
#8410 = AXIS2_PLACEMENT_3D ( 'NONE', #9808, #14612, #21469 ) ;
#8411 = STYLED_ITEM ( 'NONE', ( #10398 ), #5987 ) ;
#8412 = PRODUCT_DEFINITION_CONTEXT ( 'detailed design', #13849, 'design' ) ;
#8413 = ORIENTED_EDGE ( 'NONE', *, *, #20857, .F. ) ;
#8414 = DIRECTION ( 'NONE',  ( -1.000000000000000000, 0.000000000000000000, 0.000000000000000000 ) ) ;
#8415 = CARTESIAN_POINT ( 'NONE',  ( 28.57540678000427548, -6.776800961815481195, 13.50000000000000000 ) ) ;
#8416 = PLANE ( 'NONE',  #19970 ) ;
#8417 = ORIENTED_EDGE ( 'NONE', *, *, #7376, .F. ) ;
#8418 = CARTESIAN_POINT ( 'NONE',  ( 15.95292532278785913, -50.11873716947361856, 13.79999999999999893 ) ) ;
#8419 = ADVANCED_FACE ( 'NONE', ( #14508 ), #19791, .T. ) ;
#8420 = CARTESIAN_POINT ( 'NONE',  ( -23.29441641503749949, 3.413540866333673485, 13.50000000000000000 ) ) ;
#8421 = EDGE_CURVE ( 'NONE', #12280, #5602, #18217, .T. ) ;
#8422 = DIRECTION ( 'NONE',  ( 0.000000000000000000, 1.000000000000000000, 0.000000000000000000 ) ) ;
#8423 = CARTESIAN_POINT ( 'NONE',  ( -23.04273156199908357, 2.261510999192738680, 13.19999999999999929 ) ) ;
#8424 =( GEOMETRIC_REPRESENTATION_CONTEXT ( 3 ) GLOBAL_UNCERTAINTY_ASSIGNED_CONTEXT ( ( #11311 ) ) GLOBAL_UNIT_ASSIGNED_CONTEXT ( ( #450, #12295, #7299 ) ) REPRESENTATION_CONTEXT ( 'NONE', 'WORKASPACE' ) );
#8425 = EDGE_CURVE ( 'NONE', #15658, #1460, #2081, .T. ) ;
#8426 = LINE ( 'NONE', #15243, #15067 ) ;
#8427 = VERTEX_POINT ( 'NONE', #20464 ) ;
#8428 = TOROIDAL_SURFACE ( 'NONE', #20938, 3.200000000000003286, 0.2999999999999999889 ) ;
#8429 = VERTEX_POINT ( 'NONE', #5132 ) ;
#8430 = CIRCLE ( 'NONE', #7373, 0.04999999999999991257 ) ;
#8431 = VERTEX_POINT ( 'NONE', #20352 ) ;
#8432 = CARTESIAN_POINT ( 'NONE',  ( 29.13662752439705272, 0.000000000000000000, 1.500000000000001332 ) ) ;
#8433 = LINE ( 'NONE', #9895, #8538 ) ;
#8434 = ORIENTED_EDGE ( 'NONE', *, *, #7720, .T. ) ;
#8435 = CARTESIAN_POINT ( 'NONE',  ( 15.05356361075494576, -52.05881965543596834, 13.87239990309209325 ) ) ;
#8436 = EDGE_LOOP ( 'NONE', ( #1977, #14255, #8776, #14233 ) ) ;
#8437 =( REPRESENTATION_RELATIONSHIP ('NONE','NONE', #561, #3995 ) REPRESENTATION_RELATIONSHIP_WITH_TRANSFORMATION ( #12622 )SHAPE_REPRESENTATION_RELATIONSHIP( ) );
#8438 = EDGE_CURVE ( 'NONE', #18617, #311, #7107, .T. ) ;
#8439 = ORIENTED_EDGE ( 'NONE', *, *, #21949, .F. ) ;
#8440 = LINE ( 'NONE', #8565, #3966 ) ;
#8441 = AXIS2_PLACEMENT_3D ( 'NONE', #5799, #9032, #12681 ) ;
#8442 = AXIS2_PLACEMENT_3D ( 'NONE', #10351, #4977, #6563 ) ;
#8443 = AXIS2_PLACEMENT_3D ( 'NONE', #2628, #6763, #6123 ) ;
#8444 = CYLINDRICAL_SURFACE ( 'NONE', #13566, 0.5000000000000004441 ) ;
#8445 = ADVANCED_FACE ( 'NONE', ( #16754 ), #4602, .T. ) ;
#8446 = CARTESIAN_POINT ( 'NONE',  ( -15.95292532278785913, -52.11873716947361856, 68.00000000000000000 ) ) ;
#8447 = VECTOR ( 'NONE', #18852, 1000.000000000000000 ) ;
#8448 = VERTEX_POINT ( 'NONE', #22155 ) ;
#8449 = CARTESIAN_POINT ( 'NONE',  ( -1.724728116533986721, 42.36054587065083155, 29.66679706732590560 ) ) ;
#8450 = DIRECTION ( 'NONE',  ( 0.000000000000000000, 0.000000000000000000, -1.000000000000000000 ) ) ;
#8451 = LINE ( 'NONE', #20199, #13264 ) ;
#8452 = DIRECTION ( 'NONE',  ( 0.000000000000000000, 0.000000000000000000, 1.000000000000000000 ) ) ;
#8453 = DIRECTION ( 'NONE',  ( 0.000000000000000000, 0.000000000000000000, 1.000000000000000000 ) ) ;
#8454 = VERTEX_POINT ( 'NONE', #1532 ) ;
#8455 = CARTESIAN_POINT ( 'NONE',  ( -15.21174975910705207, 41.81054587065082728, 13.50000000000000000 ) ) ;
#8456 = EDGE_CURVE ( 'NONE', #3262, #6219, #1423, .T. ) ;
#8457 = VERTEX_POINT ( 'NONE', #3000 ) ;
#8458 = DIRECTION ( 'NONE',  ( 0.000000000000000000, 0.000000000000000000, -1.000000000000000000 ) ) ;
#8459 = CIRCLE ( 'NONE', #13462, 0.2999999999999999334 ) ;
#8460 = ORIENTED_EDGE ( 'NONE', *, *, #11793, .T. ) ;
#8461 = VECTOR ( 'NONE', #18296, 1000.000000000000000 ) ;
#8462 = VECTOR ( 'NONE', #1974, 1000.000000000000000 ) ;
#8463 = ORIENTED_EDGE ( 'NONE', *, *, #17932, .F. ) ;
#8464 = CIRCLE ( 'NONE', #578, 0.5000000000000004441 ) ;
#8465 = ORIENTED_EDGE ( 'NONE', *, *, #8534, .T. ) ;
#8466 = CARTESIAN_POINT ( 'NONE',  ( 1.724728116533979838, 43.26054587065083012, 41.71679706732590631 ) ) ;
#8467 = FACE_OUTER_BOUND ( 'NONE', #4641, .T. ) ;
#8468 = DIRECTION ( 'NONE',  ( 1.000000000000000000, -0.000000000000000000, -0.000000000000000000 ) ) ;
#8469 = EDGE_LOOP ( 'NONE', ( #20746, #5507, #5292, #5399 ) ) ;
#8470 = VECTOR ( 'NONE', #11091, 1000.000000000000000 ) ;
#8471 = VERTEX_POINT ( 'NONE', #3226 ) ;
#8472 = CARTESIAN_POINT ( 'NONE',  ( 29.13662752439705272, 0.000000000000000000, 3.500000000000000000 ) ) ;
#8473 = EDGE_CURVE ( 'NONE', #8556, #7730, #21764, .T. ) ;
#8474 = ORIENTED_EDGE ( 'NONE', *, *, #16946, .T. ) ;
#8475 = DIRECTION ( 'NONE',  ( 0.000000000000000000, 0.000000000000000000, -1.000000000000000000 ) ) ;
#8476 = VECTOR ( 'NONE', #14900, 1000.000000000000000 ) ;
#8477 = EDGE_CURVE ( 'NONE', #9810, #13749, #13393, .T. ) ;
#8478 = DIRECTION ( 'NONE',  ( -1.000000000000000000, 0.000000000000000000, 0.000000000000000000 ) ) ;
#8479 = EDGE_CURVE ( 'NONE', #6786, #14923, #8266, .T. ) ;
#8480 = CIRCLE ( 'NONE', #17389, 1.000000000000000000 ) ;
#8481 = VECTOR ( 'NONE', #15589, 1000.000000000000000 ) ;
#8482 = DIRECTION ( 'NONE',  ( 0.000000000000000000, 1.000000000000000000, 0.000000000000000000 ) ) ;
#8483 = DIRECTION ( 'NONE',  ( 1.000000000000000000, 0.000000000000000000, 0.000000000000000000 ) ) ;
#8484 = VERTEX_POINT ( 'NONE', #15179 ) ;
#8485 = CARTESIAN_POINT ( 'NONE',  ( 23.02398829872513986, 2.877181859310994572, 13.71509684061243561 ) ) ;
#8486 = LINE ( 'NONE', #15305, #7118 ) ;
#8487 = AXIS2_PLACEMENT_3D ( 'NONE', #5601, #7170, #10514 ) ;
#8488 = VECTOR ( 'NONE', #20853, 1000.000000000000000 ) ;
#8489 = LINE ( 'NONE', #13290, #16669 ) ;
#8490 = FACE_OUTER_BOUND ( 'NONE', #59, .T. ) ;
#8491 = ORIENTED_EDGE ( 'NONE', *, *, #3271, .T. ) ;
#8492 = CARTESIAN_POINT ( 'NONE',  ( -1.724728116533986721, 43.31054587065082728, 29.76679706732590702 ) ) ;
#8493 = AXIS2_PLACEMENT_3D ( 'NONE', #9814, #1291, #7927 ) ;
#8494 = DIRECTION ( 'NONE',  ( 0.000000000000000000, -1.000000000000000000, 0.000000000000000000 ) ) ;
#8495 = ORIENTED_EDGE ( 'NONE', *, *, #14486, .F. ) ;
#8496 = CARTESIAN_POINT ( 'NONE',  ( -1.824728116533986810, 43.31054587065082728, 49.76679706732591058 ) ) ;
#8497 = DIRECTION ( 'NONE',  ( -1.000000000000000000, 0.000000000000000000, 0.000000000000000000 ) ) ;
#8498 = AXIS2_PLACEMENT_3D ( 'NONE', #20124, #9610, #20018 ) ;
#8499 = AXIS2_PLACEMENT_3D ( 'NONE', #1457, #18693, #3364 ) ;
#8500 = EDGE_CURVE ( 'NONE', #5552, #573, #3443, .T. ) ;
#8501 = VERTEX_POINT ( 'NONE', #8606 ) ;
#8502 = LINE ( 'NONE', #6395, #9189 ) ;
#8503 = TOROIDAL_SURFACE ( 'NONE', #15214, 0.2999999999999999889, 0.2999999999999999889 ) ;
#8504 = ORIENTED_EDGE ( 'NONE', *, *, #7608, .F. ) ;
#8505 = ADVANCED_FACE ( 'NONE', ( #20229 ), #1374, .T. ) ;
#8506 = CARTESIAN_POINT ( 'NONE',  ( -1.724728116533986721, 43.26054587065083012, 45.76679706732590347 ) ) ;
#8507 = ORIENTED_EDGE ( 'NONE', *, *, #1844, .T. ) ;
#8508 = CARTESIAN_POINT ( 'NONE',  ( -29.26826100586361079, 2.729427995260352624, 5.717472393966525748E-18 ) ) ;
#8509 = EDGE_CURVE ( 'NONE', #11265, #15626, #3336, .T. ) ;
#8510 = DIRECTION ( 'NONE',  ( -2.832483164223434527E-16, -1.000000000000000000, 0.000000000000000000 ) ) ;
#8511 = DIRECTION ( 'NONE',  ( 1.000000000000000000, 0.000000000000000000, 0.000000000000000000 ) ) ;
#8512 = CARTESIAN_POINT ( 'NONE',  ( -14.96174975910705207, -51.61873716947361856, 68.25000000000000000 ) ) ;
#8513 = AXIS2_PLACEMENT_3D ( 'NONE', #8917, #393, #7469 ) ;
#8514 = CIRCLE ( 'NONE', #16352, 0.05000000000000143219 ) ;
#8515 = LINE ( 'NONE', #5048, #14619 ) ;
#8516 = LINE ( 'NONE', #4933, #20421 ) ;
#8517 = CARTESIAN_POINT ( 'NONE',  ( -32.23382792203229741, 83.71979900898287497, 13.74999999999999822 ) ) ;
#8518 = CARTESIAN_POINT ( 'NONE',  ( -14.71432566477614579, -52.07267295633236870, 13.50000000000000000 ) ) ;
#8519 = CARTESIAN_POINT ( 'NONE',  ( 1.724728116533979616, 42.36054587065083155, 31.70876104995653932 ) ) ;
#8520 = CIRCLE ( 'NONE', #13507, 0.5000000000000004441 ) ;
#8521 = VECTOR ( 'NONE', #10198, 1000.000000000000000 ) ;
#8522 = ORIENTED_EDGE ( 'NONE', *, *, #17317, .F. ) ;
#8523 = LINE ( 'NONE', #21953, #6349 ) ;
#8524 = DIRECTION ( 'NONE',  ( -1.000000000000000000, 0.000000000000000000, 0.000000000000000000 ) ) ;
#8525 = FACE_OUTER_BOUND ( 'NONE', #15898, .T. ) ;
#8526 = ORIENTED_EDGE ( 'NONE', *, *, #9096, .T. ) ;
#8527 = ORIENTED_EDGE ( 'NONE', *, *, #7110, .T. ) ;
#8528 = FACE_OUTER_BOUND ( 'NONE', #1596, .T. ) ;
#8529 = DIRECTION ( 'NONE',  ( 1.000000000000000000, 0.000000000000000000, 0.000000000000000000 ) ) ;
#8530 = ORIENTED_EDGE ( 'NONE', *, *, #15184, .F. ) ;
#8531 = AXIS2_PLACEMENT_3D ( 'NONE', #2708, #19730, #16571 ) ;
#8532 = AXIS2_PLACEMENT_3D ( 'NONE', #22087, #8212, #3048 ) ;
#8533 = ORIENTED_EDGE ( 'NONE', *, *, #20142, .F. ) ;
#8534 = EDGE_CURVE ( 'NONE', #4059, #19512, #21922, .T. ) ;
#8535 = ORIENTED_EDGE ( 'NONE', *, *, #21945, .F. ) ;
#8536 = EDGE_CURVE ( 'NONE', #5223, #2108, #20022, .T. ) ;
#8537 = CIRCLE ( 'NONE', #8188, 0.2500000000000002220 ) ;
#8538 = VECTOR ( 'NONE', #20300, 1000.000000000000000 ) ;
#8539 = CIRCLE ( 'NONE', #16730, 0.2500000000000002220 ) ;
#8540 = ORIENTED_EDGE ( 'NONE', *, *, #17119, .F. ) ;
#8541 = AXIS2_PLACEMENT_3D ( 'NONE', #17310, #4016, #1882 ) ;
#8542 = FACE_OUTER_BOUND ( 'NONE', #8201, .T. ) ;
#8543 = DIRECTION ( 'NONE',  ( -1.000000000000000000, 0.000000000000000000, 0.000000000000000000 ) ) ;
#8544 = CARTESIAN_POINT ( 'NONE',  ( 23.02398829872513986, 3.002822642624742855, 13.75715867294163886 ) ) ;
#8545 = CARTESIAN_POINT ( 'NONE',  ( 23.02398829872513986, -2.157133568460768647, 42.50000000000000000 ) ) ;
#8546 = DIRECTION ( 'NONE',  ( 0.9969624470112576908, -0.07788375472025980961, -0.000000000000000000 ) ) ;
#8547 = CARTESIAN_POINT ( 'NONE',  ( 0.000000000000000000, 67.54634676501045476, 7.500000000000000000 ) ) ;
#8548 = DIRECTION ( 'NONE',  ( 1.000000000000000000, 0.000000000000000000, 0.000000000000000000 ) ) ;
#8549 = AXIS2_PLACEMENT_3D ( 'NONE', #1194, #9946, #16868 ) ;
#8550 = CARTESIAN_POINT ( 'NONE',  ( -29.50000000000002132, -69.00000000000000000, -150.0833101980363722 ) ) ;
#8551 = CARTESIAN_POINT ( 'NONE',  ( 14.71479891163412468, -52.07369784467163498, 13.50000000000000178 ) ) ;
#8552 = EDGE_CURVE ( 'NONE', #18926, #17256, #11496, .T. ) ;
#8553 = CARTESIAN_POINT ( 'NONE',  ( 29.13662752439705272, 0.000000000000000000, 3.799999999999999822 ) ) ;
#8554 = ORIENTED_EDGE ( 'NONE', *, *, #700, .T. ) ;
#8555 = ORIENTED_EDGE ( 'NONE', *, *, #10842, .T. ) ;
#8556 = VERTEX_POINT ( 'NONE', #13512 ) ;
#8557 = AXIS2_PLACEMENT_3D ( 'NONE', #655, #5499, #3808 ) ;
#8558 = CARTESIAN_POINT ( 'NONE',  ( -29.26826100586361079, -2.729427995260352624, 5.717472393966525748E-18 ) ) ;
#8559 = ORIENTED_EDGE ( 'NONE', *, *, #1162, .F. ) ;
#8560 = LINE ( 'NONE', #5198, #5596 ) ;
#8561 = EDGE_CURVE ( 'NONE', #2467, #21435, #16744, .T. ) ;
#8562 = EDGE_CURVE ( 'NONE', #16140, #22083, #11596, .T. ) ;
#8563 = EDGE_CURVE ( 'NONE', #21160, #11864, #8486, .T. ) ;
#8564 = EDGE_LOOP ( 'NONE', ( #6802, #11211, #10612, #2800 ) ) ;
#8565 = CARTESIAN_POINT ( 'NONE',  ( 9.141460742840918030, -33.93424481021354921, 68.50000000000000000 ) ) ;
#8566 = FACE_OUTER_BOUND ( 'NONE', #18567, .T. ) ;
#8567 = EDGE_CURVE ( 'NONE', #13921, #4692, #18428, .T. ) ;
#8568 = DIRECTION ( 'NONE',  ( 0.000000000000000000, 0.000000000000000000, 1.000000000000000000 ) ) ;
#8569 = CIRCLE ( 'NONE', #4633, 0.2999999999999999334 ) ;
#8570 =( BOUNDED_SURFACE ( )  B_SPLINE_SURFACE ( 3, 2, ( 
 ( #17705, #12555, #16366 ),
 ( #19400, #2715, #6099 ),
 ( #5872, #4072, #2608 ),
 ( #21309, #18035, #10889 ),
 ( #1040, #7440, #11002 ),
 ( #12654, #2385, #12776 ),
 ( #21427, #14248, #19735 ),
 ( #16024, #7769, #9436 ) ),
 .UNSPECIFIED., .F., .F., .F. ) 
 B_SPLINE_SURFACE_WITH_KNOTS ( ( 4, 2, 2, 4 ),
 ( 3, 3 ),
 ( -1.707618421664669484E-18, 0.0004639257417130348096, 0.0006958886125695531088, 0.0009278514834260713539 ),
 ( 0.000000000000000000, 1.000000000000000000 ),
 .UNSPECIFIED. ) 
 GEOMETRIC_REPRESENTATION_ITEM ( )  RATIONAL_B_SPLINE_SURFACE ( (
 ( 1.000000000000000000, 0.6123724356957929160, 1.000000000000000000),
 ( 1.000000000000000000, 0.6127303078017206639, 1.000000000000000000),
 ( 1.000000000000000000, 0.6153173443167760936, 1.000000000000000000),
 ( 1.000000000000000000, 0.6312737947278392880, 1.000000000000000000),
 ( 1.000000000000000000, 0.6386439821288609764, 1.000000000000000000),
 ( 1.000000000000000000, 0.6635434878155272997, 1.000000000000000000),
 ( 1.000000000000000000, 0.6820474757551056033, 1.000000000000000000),
 ( 1.000000000000000000, 0.7071067811865495711, 1.000000000000000000) ) ) 
 REPRESENTATION_ITEM ( '' )  SURFACE ( )  );
#8571 = DIRECTION ( 'NONE',  ( -1.000000000000000000, 0.000000000000000000, 0.000000000000000000 ) ) ;
#8572 = ORIENTED_EDGE ( 'NONE', *, *, #2347, .F. ) ;
#8573 = CARTESIAN_POINT ( 'NONE',  ( -15.95292532278785913, 34.11873716947361856, 68.50000000000000000 ) ) ;
#8574 = FACE_OUTER_BOUND ( 'NONE', #5560, .T. ) ;
#8575 = LINE ( 'NONE', #20433, #21775 ) ;
#8576 = CARTESIAN_POINT ( 'NONE',  ( -3.127054932750481964, 32.61873716947361856, 68.00000000000000000 ) ) ;
#8577 =( LENGTH_UNIT ( ) NAMED_UNIT ( * ) SI_UNIT ( .MILLI., .METRE. ) );
#8578 = ORIENTED_EDGE ( 'NONE', *, *, #4846, .T. ) ;
#8579 = DIRECTION ( 'NONE',  ( -1.000000000000000000, 0.000000000000000000, -0.000000000000000000 ) ) ;
#8580 = ADVANCED_FACE ( 'NONE', ( #4904 ), #13939, .F. ) ;
#8581 = ORIENTED_EDGE ( 'NONE', *, *, #15428, .T. ) ;
#8582 = CARTESIAN_POINT ( 'NONE',  ( -23.32398829872514057, -3.528912754968629439, 13.79999999999999893 ) ) ;
#8583 = LINE ( 'NONE', #10137, #15896 ) ;
#8584 = FACE_OUTER_BOUND ( 'NONE', #5222, .T. ) ;
#8585 = VERTEX_POINT ( 'NONE', #18892 ) ;
#8586 = ORIENTED_EDGE ( 'NONE', *, *, #14136, .F. ) ;
#8587 = ORIENTED_EDGE ( 'NONE', *, *, #13523, .F. ) ;
#8588 = DIRECTION ( 'NONE',  ( 0.000000000000000000, -0.000000000000000000, -1.000000000000000000 ) ) ;
#8589 = DIRECTION ( 'NONE',  ( 0.000000000000000000, 0.000000000000000000, -1.000000000000000000 ) ) ;
#8590 = DIRECTION ( 'NONE',  ( -0.000000000000000000, -0.000000000000000000, 1.000000000000000000 ) ) ;
#8591 = AXIS2_PLACEMENT_3D ( 'NONE', #8699, #7132, #17513 ) ;
#8592 = ORIENTED_EDGE ( 'NONE', *, *, #18143, .T. ) ;
#8593 = CARTESIAN_POINT ( 'NONE',  ( -1.824728116533986810, 43.31054587065082728, 43.80876104995653719 ) ) ;
#8594 = ADVANCED_FACE ( 'NONE', ( #19324 ), #2305, .T. ) ;
#8595 = EDGE_LOOP ( 'NONE', ( #14621, #698, #21266, #19958, #19037, #13576, #9093, #17072 ) ) ;
#8596 = DIRECTION ( 'NONE',  ( 1.000000000000000000, 0.000000000000000000, 0.000000000000000000 ) ) ;
#8597 = EDGE_CURVE ( 'NONE', #7888, #16845, #7471, .T. ) ;
#8598 = B_SPLINE_CURVE_WITH_KNOTS ( 'NONE', 3,
 ( #5922, #16186, #11163, #1096 ),
 .UNSPECIFIED., .F., .F.,
 ( 4, 4 ),
 ( 0.005071647684206891105, 0.007900577432593609145 ),
 .UNSPECIFIED. ) ;
#8599 = VERTEX_POINT ( 'NONE', #3566 ) ;
#8600 = CARTESIAN_POINT ( 'NONE',  ( -21.71259690522456154, 45.22582864897715638, 13.50000000000000000 ) ) ;
#8601 = CARTESIAN_POINT ( 'NONE',  ( -9.641460742840918030, 32.61873716947361856, 68.50000000000000000 ) ) ;
#8602 = CARTESIAN_POINT ( 'NONE',  ( -32.23382792203229741, 83.71979900898287497, 68.25000000000000000 ) ) ;
#8603 = DIRECTION ( 'NONE',  ( 1.000000000000000000, 0.000000000000000000, 0.000000000000000000 ) ) ;
#8604 = ORIENTED_EDGE ( 'NONE', *, *, #5348, .T. ) ;
#8605 = CARTESIAN_POINT ( 'NONE',  ( 23.02398829872513986, 2.624244922594596741, 13.63058196926744792 ) ) ;
#8606 = CARTESIAN_POINT ( 'NONE',  ( -23.32398829872514057, -5.683640910026986681, 13.50000000000000000 ) ) ;
#8607 = AXIS2_PLACEMENT_3D ( 'NONE', #2678, #15990, #14422 ) ;
#8608 = AXIS2_PLACEMENT_3D ( 'NONE', #8100, #1245, #9548 ) ;
#8609 = DIRECTION ( 'NONE',  ( -0.2309407893631976738, 0.9729678061520347088, 0.000000000000000000 ) ) ;
#8610 = CYLINDRICAL_SURFACE ( 'NONE', #2468, 0.3000000000000016542 ) ;
#8611 = VERTEX_POINT ( 'NONE', #9135 ) ;
#8612 = FACE_OUTER_BOUND ( 'NONE', #19198, .T. ) ;
#8613 = FACE_OUTER_BOUND ( 'NONE', #15012, .T. ) ;
#8614 = ORIENTED_EDGE ( 'NONE', *, *, #3826, .T. ) ;
#8615 = DIRECTION ( 'NONE',  ( 1.000000000000000000, 0.000000000000000000, -0.000000000000000000 ) ) ;
#8616 = EDGE_CURVE ( 'NONE', #7158, #17039, #88, .T. ) ;
#8617 = DIRECTION ( 'NONE',  ( 8.326672684688666480E-14, 0.000000000000000000, 1.000000000000000000 ) ) ;
#8618 = EDGE_CURVE ( 'NONE', #21526, #14178, #14155, .T. ) ;
#8619 = ORIENTED_EDGE ( 'NONE', *, *, #13873, .T. ) ;
#8620 = CARTESIAN_POINT ( 'NONE',  ( -26.61833302554978786, -9.663695060508651125, 13.50000000000000000 ) ) ;
#8621 = AXIS2_PLACEMENT_3D ( 'NONE', #13152, #16269, #7812 ) ;
#8622 = AXIS2_PLACEMENT_3D ( 'NONE', #5412, #348, #9082 ) ;
#8623 = ORIENTED_EDGE ( 'NONE', *, *, #7683, .F. ) ;
#8624 = EDGE_CURVE ( 'NONE', #17966, #16219, #21047, .T. ) ;
#8625 = LINE ( 'NONE', #16151, #10253 ) ;
#8626 = EDGE_LOOP ( 'NONE', ( #18958, #1572, #2705, #5837 ) ) ;
#8627 = DIRECTION ( 'NONE',  ( 1.000000000000000000, 0.000000000000000000, 0.000000000000000000 ) ) ;
#8628 = LINE ( 'NONE', #11847, #19719 ) ;
#8629 = DIRECTION ( 'NONE',  ( 0.000000000000000000, 0.000000000000000000, -1.000000000000000000 ) ) ;
#8630 = AXIS2_PLACEMENT_3D ( 'NONE', #4679, #18417, #6484 ) ;
#8631 = PLANE ( 'NONE',  #12271 ) ;
#8632 = CARTESIAN_POINT ( 'NONE',  ( -15.21174975910705385, -52.00603550409435627, 13.50000000000000000 ) ) ;
#8633 = VERTEX_POINT ( 'NONE', #7147 ) ;
#8634 = EDGE_CURVE ( 'NONE', #1458, #5468, #8537, .T. ) ;
#8635 = DIRECTION ( 'NONE',  ( 0.000000000000000000, -0.000000000000000000, -1.000000000000000000 ) ) ;
#8636 = FACE_BOUND ( 'NONE', #15613, .T. ) ;
#8637 = CIRCLE ( 'NONE', #752, 1.000000000000000888 ) ;
#8638 = DIRECTION ( 'NONE',  ( -0.000000000000000000, -0.000000000000000000, -1.000000000000000000 ) ) ;
#8639 = ADVANCED_FACE ( 'NONE', ( #5362 ), #22122, .T. ) ;
#8640 = CIRCLE ( 'NONE', #11841, 0.05000000000000143219 ) ;
#8641 = VERTEX_POINT ( 'NONE', #5471 ) ;
#8642 = ORIENTED_EDGE ( 'NONE', *, *, #5619, .T. ) ;
#8643 = FACE_OUTER_BOUND ( 'NONE', #5968, .T. ) ;
#8644 = DIRECTION ( 'NONE',  ( 1.000000000000000000, 0.000000000000000000, 0.000000000000000000 ) ) ;
#8645 = CIRCLE ( 'NONE', #6157, 0.04999999999999991257 ) ;
#8646 = EDGE_LOOP ( 'NONE', ( #13023, #17334, #20722, #15523 ) ) ;
#8647 = AXIS2_PLACEMENT_3D ( 'NONE', #14798, #20177, #14579 ) ;
#8648 = FILL_AREA_STYLE_COLOUR ( '', #20375 ) ;
#8649 = VERTEX_POINT ( 'NONE', #2088 ) ;
#8650 = ORIENTED_EDGE ( 'NONE', *, *, #6241, .T. ) ;
#8651 = VERTEX_POINT ( 'NONE', #5699 ) ;
#8652 = DIRECTION ( 'NONE',  ( 1.000000000000000000, 0.000000000000000000, 0.000000000000000000 ) ) ;
#8653 = DIRECTION ( 'NONE',  ( 0.000000000000000000, 0.000000000000000000, -1.000000000000000000 ) ) ;
#8654 = ADVANCED_FACE ( 'NONE', ( #8713 ), #6758, .T. ) ;
#8655 = PLANE ( 'NONE',  #13164 ) ;
#8656 = DIRECTION ( 'NONE',  ( 0.07788375472025979573, 0.9969624470112574688, 0.000000000000000000 ) ) ;
#8657 = AXIS2_PLACEMENT_3D ( 'NONE', #2145, #4155, #7418 ) ;
#8658 = DIRECTION ( 'NONE',  ( 0.000000000000000000, 0.000000000000000000, 1.000000000000000000 ) ) ;
#8659 = AXIS2_PLACEMENT_3D ( 'NONE', #1991, #12274, #10411 ) ;
#8660 = DIRECTION ( 'NONE',  ( 0.000000000000000000, 1.000000000000000000, 0.000000000000000000 ) ) ;
#8661 = CARTESIAN_POINT ( 'NONE',  ( 23.08512718742729319, -2.485300415563061360, 13.35387015137019873 ) ) ;
#8662 = DIRECTION ( 'NONE',  ( -1.000000000000000000, 0.000000000000000000, -0.000000000000000000 ) ) ;
#8663 = AXIS2_PLACEMENT_3D ( 'NONE', #9404, #14420, #21272 ) ;
#8664 = ADVANCED_FACE ( 'NONE', ( #10819 ), #15508, .T. ) ;
#8665 = CARTESIAN_POINT ( 'NONE',  ( -1.724728116533986721, 43.26054587065083012, 37.76679706732590347 ) ) ;
#8666 = ORIENTED_EDGE ( 'NONE', *, *, #6517, .F. ) ;
#8667 = ORIENTED_EDGE ( 'NONE', *, *, #15976, .T. ) ;
#8668 = CARTESIAN_POINT ( 'NONE',  ( -31.01761816434227015, 84.00847499568689614, 68.25000000000000000 ) ) ;
#8669 = SURFACE_SIDE_STYLE ('',( #1926 ) ) ;
#8670 = DIRECTION ( 'NONE',  ( -0.000000000000000000, -1.000000000000000000, -0.000000000000000000 ) ) ;
#8671 = VERTEX_POINT ( 'NONE', #13828 ) ;
#8672 = B_SPLINE_CURVE_WITH_KNOTS ( 'NONE', 3,
 ( #6440, #11880, #20080, #1248, #8104, #16697 ),
 .UNSPECIFIED., .F., .F.,
 ( 4, 2, 4 ),
 ( 0.000000000000000000, 0.0002343433793794306779, 0.0004686867587588613559 ),
 .UNSPECIFIED. ) ;
#8673 = VECTOR ( 'NONE', #1197, 1000.000000000000000 ) ;
#8674 = CIRCLE ( 'NONE', #4739, 0.2500000000000002220 ) ;
#8675 = DIRECTION ( 'NONE',  ( 0.000000000000000000, 1.000000000000000000, 0.000000000000000000 ) ) ;
#8676 = ADVANCED_FACE ( 'NONE', ( #3671 ), #8923, .F. ) ;
#8677 = DIRECTION ( 'NONE',  ( 0.000000000000000000, -0.000000000000000000, -1.000000000000000000 ) ) ;
#8678 = CARTESIAN_POINT ( 'NONE',  ( -34.40000000000001279, -84.70000000000001705, 79.70000000000000284 ) ) ;
#8679 = ORIENTED_EDGE ( 'NONE', *, *, #16015, .F. ) ;
#8680 = CYLINDRICAL_SURFACE ( 'NONE', #10956, 0.1000000000000028644 ) ;
#8681 = CIRCLE ( 'NONE', #9045, 0.2999999999999999334 ) ;
#8682 = DIRECTION ( 'NONE',  ( 0.000000000000000000, 0.000000000000000000, 1.000000000000000000 ) ) ;
#8683 = CYLINDRICAL_SURFACE ( 'NONE', #21171, 0.5000000000000004441 ) ;
#8684 = CARTESIAN_POINT ( 'NONE',  ( -1.774728116533986766, 42.31054587065082728, 8.000000000000000000 ) ) ;
#8685 = DIRECTION ( 'NONE',  ( -0.000000000000000000, 1.000000000000000000, -0.000000000000000000 ) ) ;
#8686 = DIRECTION ( 'NONE',  ( 0.000000000000000000, 1.000000000000000000, 0.000000000000000000 ) ) ;
#8687 = DIRECTION ( 'NONE',  ( -0.000000000000000000, 0.000000000000000000, -1.000000000000000000 ) ) ;
#8688 = DIRECTION ( 'NONE',  ( -0.000000000000000000, 1.000000000000000000, -0.000000000000000000 ) ) ;
#8689 = ADVANCED_FACE ( 'NONE', ( #15614 ), #296, .F. ) ;
#8690 = ORIENTED_EDGE ( 'NONE', *, *, #11376, .F. ) ;
#8691 = DIRECTION ( 'NONE',  ( 0.000000000000000000, -0.000000000000000000, -1.000000000000000000 ) ) ;
#8692 = CARTESIAN_POINT ( 'NONE',  ( 0.000000000000000000, -38.74634676501045760, 42.50000000000000000 ) ) ;
#8693 = ADVANCED_FACE ( 'NONE', ( #400 ), #20896, .F. ) ;
#8694 = ORIENTED_EDGE ( 'NONE', *, *, #775, .T. ) ;
#8695 = VERTEX_POINT ( 'NONE', #505 ) ;
#8696 = ORIENTED_EDGE ( 'NONE', *, *, #4772, .T. ) ;
#8697 = DIRECTION ( 'NONE',  ( -1.000000000000000000, 0.000000000000000000, 0.000000000000000000 ) ) ;
#8698 = FACE_OUTER_BOUND ( 'NONE', #10695, .T. ) ;
#8699 = CARTESIAN_POINT ( 'NONE',  ( -1.724728116533986721, 42.31054587065082728, 45.66679706732590205 ) ) ;
#8700 = ADVANCED_FACE ( 'NONE', ( #16396 ), #10668, .F. ) ;
#8701 = DIRECTION ( 'NONE',  ( 0.000000000000000000, 0.000000000000000000, 1.000000000000000000 ) ) ;
#8702 = B_SPLINE_CURVE_WITH_KNOTS ( 'NONE', 3,
 ( #14860, #16646, #18338, #13528, #13301, #3014, #9844, #1325 ),
 .UNSPECIFIED., .F., .F.,
 ( 4, 2, 2, 4 ),
 ( 3.388890645555526065E-18, 0.0001462888802157341281, 0.0002925777604314648951, 0.0005851555208629193820 ),
 .UNSPECIFIED. ) ;
#8703 = VERTEX_POINT ( 'NONE', #7914 ) ;
#8704 = FACE_OUTER_BOUND ( 'NONE', #15762, .T. ) ;
#8705 = ADVANCED_FACE ( 'NONE', ( #11359 ), #5800, .T. ) ;
#8706 = ORIENTED_EDGE ( 'NONE', *, *, #14731, .F. ) ;
#8707 = DIRECTION ( 'NONE',  ( -0.000000000000000000, -0.000000000000000000, -1.000000000000000000 ) ) ;
#8708 = DIRECTION ( 'NONE',  ( 0.000000000000000000, -1.000000000000000000, 0.000000000000000000 ) ) ;
#8709 = CARTESIAN_POINT ( 'NONE',  ( -29.69597781366221767, 58.69165929845684815, 70.25000000000000000 ) ) ;
#8710 = DIRECTION ( 'NONE',  ( -1.000000000000000000, 0.000000000000000000, 0.000000000000000000 ) ) ;
#8711 = ORIENTED_EDGE ( 'NONE', *, *, #10865, .T. ) ;
#8712 = CARTESIAN_POINT ( 'NONE',  ( 25.37540678000427263, -63.74634676501045050, 7.500000000000000000 ) ) ;
#8713 = FACE_OUTER_BOUND ( 'NONE', #4499, .T. ) ;
#8714 = DIRECTION ( 'NONE',  ( -1.000000000000000000, 0.000000000000000000, 0.000000000000000000 ) ) ;
#8715 = DIRECTION ( 'NONE',  ( 0.000000000000000000, -1.000000000000000000, 0.000000000000000000 ) ) ;
#8716 = ORIENTED_EDGE ( 'NONE', *, *, #5290, .T. ) ;
#8717 = CARTESIAN_POINT ( 'NONE',  ( 1.724728116533979838, 43.26054587065083012, 33.66679706732590915 ) ) ;
#8718 = EDGE_CURVE ( 'NONE', #12023, #21932, #15652, .T. ) ;
#8719 = EDGE_CURVE ( 'NONE', #2819, #2099, #19974, .T. ) ;
#8720 = CARTESIAN_POINT ( 'NONE',  ( 29.37540678000427619, 5.000000000000000000, 7.200000000000000178 ) ) ;
#8721 = ORIENTED_EDGE ( 'NONE', *, *, #18542, .T. ) ;
#8723 = EDGE_CURVE ( 'NONE', #13403, #16971, #1005, .T. ) ;
#8722 = CARTESIAN_POINT ( 'NONE',  ( 32.20000000000001705, 71.00000000000001421, 1.800000000000000044 ) ) ;
#8724 = ORIENTED_EDGE ( 'NONE', *, *, #8985, .T. ) ;
#8725 = ORIENTED_EDGE ( 'NONE', *, *, #16712, .F. ) ;
#8726 = EDGE_CURVE ( 'NONE', #15395, #11905, #12434, .T. ) ;
#8727 = EDGE_LOOP ( 'NONE', ( #13446, #1941, #13352, #19804 ) ) ;
#8728 = CARTESIAN_POINT ( 'NONE',  ( -29.20000000000002061, 2.799282752659324025, 0.000000000000000000 ) ) ;
#8729 = AXIS2_PLACEMENT_3D ( 'NONE', #8517, #15207, #5159 ) ;
#8730 = AXIS2_PLACEMENT_3D ( 'NONE', #2011, #3488, #6866 ) ;
#8731 = CARTESIAN_POINT ( 'NONE',  ( -6.728906393579157097, 41.92645089659919933, 70.88527860057354246 ) ) ;
#8732 = DIRECTION ( 'NONE',  ( 0.000000000000000000, 0.000000000000000000, 1.000000000000000000 ) ) ;
#8733 = EDGE_CURVE ( 'NONE', #22148, #879, #15317, .T. ) ;
#8734 = UNCERTAINTY_MEASURE_WITH_UNIT (LENGTH_MEASURE( 1.000000000000000082E-05 ), #6199, 'distance_accuracy_value', 'NONE');
#8735 = DIRECTION ( 'NONE',  ( 0.000000000000000000, 1.000000000000000000, 0.000000000000000000 ) ) ;
#8736 = CARTESIAN_POINT ( 'NONE',  ( 1.724728116533979616, 42.31054587065082728, 37.71679706732590631 ) ) ;
#8737 = CARTESIAN_POINT ( 'NONE',  ( -31.50000000000002132, -72.00000000000001421, 3.200000000000000178 ) ) ;
#8738 = EDGE_CURVE ( 'NONE', #22039, #21353, #2527, .T. ) ;
#8739 = ORIENTED_EDGE ( 'NONE', *, *, #1344, .F. ) ;
#8740 = CARTESIAN_POINT ( 'NONE',  ( 15.95292532278785913, -50.11873716947361856, 13.50000000000000000 ) ) ;
#8741 = DIRECTION ( 'NONE',  ( 0.000000000000000000, 0.000000000000000000, -1.000000000000000000 ) ) ;
#8742 = DIRECTION ( 'NONE',  ( -1.000000000000000000, -0.000000000000000000, -0.000000000000000000 ) ) ;
#8743 = VERTEX_POINT ( 'NONE', #15939 ) ;
#8744 = ORIENTED_EDGE ( 'NONE', *, *, #12875, .F. ) ;
#8745 = DIRECTION ( 'NONE',  ( -0.000000000000000000, 1.000000000000000000, 0.000000000000000000 ) ) ;
#8746 = APPLICATION_PROTOCOL_DEFINITION ( 'draft international standard', 'automotive_design', 1998, #1985 ) ;
#8747 = VERTEX_POINT ( 'NONE', #18063 ) ;
#8748 = CARTESIAN_POINT ( 'NONE',  ( 23.02398829872514341, -2.279831973701432535, 13.43058255391203382 ) ) ;
#8749 = EDGE_LOOP ( 'NONE', ( #7181, #1226, #14833, #12544 ) ) ;
#8750 = ORIENTED_EDGE ( 'NONE', *, *, #7022, .F. ) ;
#8751 = ADVANCED_FACE ( 'NONE', ( #4537 ), #11238, .T. ) ;
#8752 = FACE_OUTER_BOUND ( 'NONE', #20877, .T. ) ;
#8753 = FACE_OUTER_BOUND ( 'NONE', #3427, .T. ) ;
#8754 = EDGE_CURVE ( 'NONE', #7977, #7598, #10002, .T. ) ;
#8755 = DIRECTION ( 'NONE',  ( -1.000000000000000000, 0.000000000000000000, 0.000000000000000000 ) ) ;
#8756 = AXIS2_PLACEMENT_3D ( 'NONE', #5640, #17148, #18831 ) ;
#8757 = DIRECTION ( 'NONE',  ( 0.000000000000000000, -1.000000000000000000, 0.000000000000000000 ) ) ;
#8758 = DIRECTION ( 'NONE',  ( 0.000000000000000000, 1.000000000000000000, 0.000000000000000000 ) ) ;
#8759 = LINE ( 'NONE', #5754, #5074 ) ;
#8760 = DIRECTION ( 'NONE',  ( -0.000000000000000000, -0.000000000000000000, 1.000000000000000000 ) ) ;
#8761 = CARTESIAN_POINT ( 'NONE',  ( 15.95292532278785913, 50.11873716947361856, 13.99999999999999822 ) ) ;
#8762 = CARTESIAN_POINT ( 'NONE',  ( 0.000000000000000000, -32.11873716947361856, 42.50000000000000711 ) ) ;
#8763 = ORIENTED_EDGE ( 'NONE', *, *, #16402, .F. ) ;
#8764 = ORIENTED_EDGE ( 'NONE', *, *, #17401, .T. ) ;
#8765 = LINE ( 'NONE', #14103, #17094 ) ;
#8766 = FILL_AREA_STYLE ('',( #10347 ) ) ;
#8767 = DIRECTION ( 'NONE',  ( 0.000000000000000000, -0.000000000000000000, -1.000000000000000000 ) ) ;
#8768 = ORIENTED_EDGE ( 'NONE', *, *, #17150, .T. ) ;
#8769 = EDGE_CURVE ( 'NONE', #3678, #14823, #4323, .T. ) ;
#8770 = VECTOR ( 'NONE', #10723, 1000.000000000000000 ) ;
#8771 = COLOUR_RGB ( '', 0.66274510, 0.83137255, 0.94901961) ;
#8772 = EDGE_CURVE ( 'NONE', #14847, #17942, #8203, .T. ) ;
#8773 = DIRECTION ( 'NONE',  ( 0.000000000000000000, 0.000000000000000000, 1.000000000000000000 ) ) ;
#8774 = DIRECTION ( 'NONE',  ( -0.000000000000000000, -0.000000000000000000, 1.000000000000000000 ) ) ;
#8775 = VECTOR ( 'NONE', #15171, 1000.000000000000000 ) ;
#8776 = ORIENTED_EDGE ( 'NONE', *, *, #7605, .T. ) ;
#8777 = CARTESIAN_POINT ( 'NONE',  ( 1.724728116533979838, 43.31054587065082728, 37.66679706732590915 ) ) ;
#8778 = DIRECTION ( 'NONE',  ( 0.000000000000000000, 0.000000000000000000, 1.000000000000000000 ) ) ;
#8779 = CYLINDRICAL_SURFACE ( 'NONE', #16017, 0.2500000000000001665 ) ;
#8780 = DIRECTION ( 'NONE',  ( 1.000000000000000000, -0.000000000000000000, 0.000000000000000000 ) ) ;
#8781 = CYLINDRICAL_SURFACE ( 'NONE', #8318, 4.575000000000001066 ) ;
#8782 = DIRECTION ( 'NONE',  ( -0.000000000000000000, -0.000000000000000000, 1.000000000000000000 ) ) ;
#8783 = VECTOR ( 'NONE', #17713, 1000.000000000000000 ) ;
#8784 = CIRCLE ( 'NONE', #16622, 0.1000000000000028644 ) ;
#8785 = CIRCLE ( 'NONE', #4494, 2.500000000000000444 ) ;
#8786 = ORIENTED_EDGE ( 'NONE', *, *, #17275, .T. ) ;
#8787 = CARTESIAN_POINT ( 'NONE',  ( 31.44597781366222122, 0.000000000000000000, 70.25000000000000000 ) ) ;
#8788 = CARTESIAN_POINT ( 'NONE',  ( -1.724728116533986721, 42.36054587065083155, 27.80876104995653719 ) ) ;
#8789 = CARTESIAN_POINT ( 'NONE',  ( 9.641460742840918030, 32.93424481021354921, 68.50000000000000000 ) ) ;
#8790 = VERTEX_POINT ( 'NONE', #2633 ) ;
#8791 = ORIENTED_EDGE ( 'NONE', *, *, #4576, .T. ) ;
#8792 = ORIENTED_EDGE ( 'NONE', *, *, #1405, .F. ) ;
#8793 = CARTESIAN_POINT ( 'NONE',  ( 17.95292532278785913, -34.11873716947361856, 42.50000000000000711 ) ) ;
#8794 = CYLINDRICAL_SURFACE ( 'NONE', #1343, 0.2999999999999999889 ) ;
#8795 = EDGE_CURVE ( 'NONE', #9891, #18983, #14378, .T. ) ;
#8796 = CIRCLE ( 'NONE', #8441, 5.000000000000004441 ) ;
#8797 = VECTOR ( 'NONE', #17103, 1000.000000000000000 ) ;
#8798 = DIRECTION ( 'NONE',  ( -0.000000000000000000, 0.000000000000000000, 1.000000000000000000 ) ) ;
#8799 = AXIS2_PLACEMENT_3D ( 'NONE', #6010, #12799, #4318 ) ;
#8800 = ORIENTED_EDGE ( 'NONE', *, *, #7093, .F. ) ;
#8801 = CARTESIAN_POINT ( 'NONE',  ( -28.87540678000427619, 63.74634676501045050, 7.799999999999999822 ) ) ;
#8802 = VECTOR ( 'NONE', #10532, 1000.000000000000000 ) ;
#8803 = EDGE_CURVE ( 'NONE', #2243, #5056, #19621, .T. ) ;
#8804 = ORIENTED_EDGE ( 'NONE', *, *, #8616, .T. ) ;
#8805 = CARTESIAN_POINT ( 'NONE',  ( -23.29450335057350330, -3.413880037201929341, 13.50000000000000178 ) ) ;
#8806 = ADVANCED_FACE ( 'NONE', ( #1067 ), #7801, .T. ) ;
#8807 = DIRECTION ( 'NONE',  ( -1.000000000000000000, 0.000000000000000000, 0.000000000000000000 ) ) ;
#8808 = CARTESIAN_POINT ( 'NONE',  ( 15.21174975910707161, 41.81054587065082728, 68.50000000000000000 ) ) ;
#8809 = DIRECTION ( 'NONE',  ( -1.000000000000000000, 0.000000000000000000, 0.000000000000000000 ) ) ;
#8810 = ORIENTED_EDGE ( 'NONE', *, *, #2502, .T. ) ;
#8811 = CARTESIAN_POINT ( 'NONE',  ( 23.02398829872513986, 2.279872152331596347, 13.43073953831959066 ) ) ;
#8812 = CARTESIAN_POINT ( 'NONE',  ( -1.774728116533986766, 42.36054587065083155, 47.70876104995654288 ) ) ;
#8813 = FACE_OUTER_BOUND ( 'NONE', #5144, .T. ) ;
#8814 = DIRECTION ( 'NONE',  ( -1.000000000000000000, 0.000000000000000000, 0.000000000000000000 ) ) ;
#8815 = VERTEX_POINT ( 'NONE', #21458 ) ;
#8816 = CIRCLE ( 'NONE', #1659, 0.3000000000000016542 ) ;
#8817 = CIRCLE ( 'NONE', #12363, 0.2999999999999999334 ) ;
#8818 = SURFACE_STYLE_FILL_AREA ( #12156 ) ;
#8819 = CIRCLE ( 'NONE', #16292, 4.700000000000002842 ) ;
#8820 = VERTEX_POINT ( 'NONE', #7679 ) ;
#8821 = CYLINDRICAL_SURFACE ( 'NONE', #21325, 0.2999999999999999334 ) ;
#8822 = EDGE_LOOP ( 'NONE', ( #3246, #6864, #16176, #16793 ) ) ;
#8823 = VECTOR ( 'NONE', #3261, 1000.000000000000000 ) ;
#8824 = ORIENTED_EDGE ( 'NONE', *, *, #18932, .T. ) ;
#8825 = DIRECTION ( 'NONE',  ( 0.000000000000000000, 0.000000000000000000, -1.000000000000000000 ) ) ;
#8826 = EDGE_CURVE ( 'NONE', #1412, #13878, #14478, .T. ) ;
#8827 = LINE ( 'NONE', #19229, #7083 ) ;
#8828 = EDGE_LOOP ( 'NONE', ( #8941, #9984, #19084, #16944 ) ) ;
#8829 = ORIENTED_EDGE ( 'NONE', *, *, #4834, .T. ) ;
#8830 = AXIS2_PLACEMENT_3D ( 'NONE', #9347, #10706, #19524 ) ;
#8831 = VECTOR ( 'NONE', #18062, 1000.000000000000000 ) ;
#8832 = VECTOR ( 'NONE', #19564, 1000.000000000000000 ) ;
#8833 = ORIENTED_EDGE ( 'NONE', *, *, #4167, .T. ) ;
#8834 = CARTESIAN_POINT ( 'NONE',  ( 15.95292532278785913, 34.11873716947361856, 68.00000000000000000 ) ) ;
#8835 = ADVANCED_FACE ( 'NONE', ( #3306 ), #2831, .T. ) ;
#8836 = AXIS2_PLACEMENT_3D ( 'NONE', #11806, #20668, #72 ) ;
#8837 = CYLINDRICAL_SURFACE ( 'NONE', #12202, 0.3000000000000016542 ) ;
#8838 = EDGE_CURVE ( 'NONE', #12241, #9450, #11048, .T. ) ;
#8839 = CARTESIAN_POINT ( 'NONE',  ( 1.824728116533979261, 42.36054587065083155, 43.80876104995653719 ) ) ;
#8840 = ORIENTED_EDGE ( 'NONE', *, *, #13531, .T. ) ;
#8841 = CARTESIAN_POINT ( 'NONE',  ( 15.21174975910705918, 52.39333383871510108, 13.50000000000000000 ) ) ;
#8842 = DIRECTION ( 'NONE',  ( 1.000000000000000000, 0.000000000000000000, 0.000000000000000000 ) ) ;
#8843 = CARTESIAN_POINT ( 'NONE',  ( 23.32398829872514057, 2.157133568460765538, 7.500000000000000000 ) ) ;
#8844 = AXIS2_PLACEMENT_3D ( 'NONE', #15427, #10404, #13728 ) ;
#8845 = AXIS2_PLACEMENT_3D ( 'NONE', #10952, #12400, #15763 ) ;
#8846 = VERTEX_POINT ( 'NONE', #13255 ) ;
#8847 = EDGE_CURVE ( 'NONE', #21631, #1527, #1036, .T. ) ;
#8848 = CYLINDRICAL_SURFACE ( 'NONE', #21361, 0.05000000000000143219 ) ;
#8849 = TOROIDAL_SURFACE ( 'NONE', #3851, 0.05000000000000000278, 0.05000000000000000278 ) ;
#8850 = ORIENTED_EDGE ( 'NONE', *, *, #14440, .T. ) ;
#8851 = VECTOR ( 'NONE', #2511, 1000.000000000000000 ) ;
#8852 = EDGE_LOOP ( 'NONE', ( #17915, #5424, #6271 ) ) ;
#8853 = DIRECTION ( 'NONE',  ( 0.000000000000000000, 0.000000000000000000, 1.000000000000000000 ) ) ;
#8854 = AXIS2_PLACEMENT_3D ( 'NONE', #15281, #5116, #11916 ) ;
#8855 =( LENGTH_UNIT ( ) NAMED_UNIT ( * ) SI_UNIT ( .MILLI., .METRE. ) );
#8856 = ORIENTED_EDGE ( 'NONE', *, *, #8534, .F. ) ;
#8857 = DIRECTION ( 'NONE',  ( 0.000000000000000000, 0.000000000000000000, 1.000000000000000000 ) ) ;
#8858 = ORIENTED_EDGE ( 'NONE', *, *, #20828, .T. ) ;
#8859 = EDGE_CURVE ( 'NONE', #5394, #17668, #2102, .T. ) ;
#8860 = VECTOR ( 'NONE', #11843, 1000.000000000000000 ) ;
#8861 = VECTOR ( 'NONE', #16964, 1000.000000000000000 ) ;
#8862 = AXIS2_PLACEMENT_3D ( 'NONE', #1883, #20530, #10169 ) ;
#8863 = ORIENTED_EDGE ( 'NONE', *, *, #11828, .T. ) ;
#8864 = ADVANCED_FACE ( 'NONE', ( #4988 ), #3195, .T. ) ;
#8865 = CYLINDRICAL_SURFACE ( 'NONE', #15910, 0.2999999999999999334 ) ;
#8866 = DIRECTION ( 'NONE',  ( 0.000000000000000000, 0.000000000000000000, -1.000000000000000000 ) ) ;
#8867 = DIRECTION ( 'NONE',  ( -1.000000000000000000, 0.000000000000000000, 0.000000000000000000 ) ) ;
#8868 = AXIS2_PLACEMENT_3D ( 'NONE', #4927, #16777, #5154 ) ;
#8869 = LINE ( 'NONE', #1914, #20755 ) ;
#8870 = TOROIDAL_SURFACE ( 'NONE', #20306, 0.05000000000000000278, 0.05000000000000000278 ) ;
#8871 =( REPRESENTATION_RELATIONSHIP ('NONE','NONE', #561, #10840 ) REPRESENTATION_RELATIONSHIP_WITH_TRANSFORMATION ( #9290 )SHAPE_REPRESENTATION_RELATIONSHIP( ) );
#8872 = CARTESIAN_POINT ( 'NONE',  ( 34.69999999999998863, -85.00000000000000000, 79.39999999999999147 ) ) ;
#8873 = DIRECTION ( 'NONE',  ( 0.000000000000000000, -1.000000000000000000, 0.000000000000000000 ) ) ;
#8874 = CARTESIAN_POINT ( 'NONE',  ( 23.04709339880124475, -2.285361808764056590, 13.25160309052396279 ) ) ;
#8875 = DIRECTION ( 'NONE',  ( 0.000000000000000000, 0.000000000000000000, 1.000000000000000000 ) ) ;
#8876 = LINE ( 'NONE', #5526, #410 ) ;
#8877 = VECTOR ( 'NONE', #12911, 1000.000000000000000 ) ;
#8878 = VECTOR ( 'NONE', #2024, 1000.000000000000114 ) ;
#8879 = ORIENTED_EDGE ( 'NONE', *, *, #13893, .T. ) ;
#8880 = EDGE_LOOP ( 'NONE', ( #21856, #21960, #3733 ) ) ;
#8881 = CARTESIAN_POINT ( 'NONE',  ( -9.718906393579157310, 43.26651812033729527, 68.06527860057354928 ) ) ;
#8883 = ADVANCED_FACE ( 'NONE', ( #1505 ), #21996, .F. ) ;
#8882 = CARTESIAN_POINT ( 'NONE',  ( -21.92816239687475743, 42.46645089659918426, 68.25000000000000000 ) ) ;
#8884 = ORIENTED_EDGE ( 'NONE', *, *, #8477, .T. ) ;
#8885 = ADVANCED_FACE ( 'NONE', ( #10025 ), #2973, .F. ) ;
#8886 = AXIS2_PLACEMENT_3D ( 'NONE', #7287, #10752, #19039 ) ;
#8887 = AXIS2_PLACEMENT_3D ( 'NONE', #20363, #5139, #8615 ) ;
#8888 = FACE_OUTER_BOUND ( 'NONE', #11254, .T. ) ;
#8889 = AXIS2_PLACEMENT_3D ( 'NONE', #1771, #20356, #10598 ) ;
#8890 = LINE ( 'NONE', #3970, #5604 ) ;
#8891 = VERTEX_POINT ( 'NONE', #16598 ) ;
#8892 = DIRECTION ( 'NONE',  ( 0.000000000000000000, 0.000000000000000000, 1.000000000000000000 ) ) ;
#8893 = CARTESIAN_POINT ( 'NONE',  ( -15.95292532278785913, -32.61873716947361856, 68.00000000000000000 ) ) ;
#8894 = LINE ( 'NONE', #2272, #5426 ) ;
#8895 = AXIS2_PLACEMENT_3D ( 'NONE', #3077, #6462, #9698 ) ;
#8896 = PLANE ( 'NONE',  #15692 ) ;
#8897 = CARTESIAN_POINT ( 'NONE',  ( 0.000000000000000000, 43.26054587065083012, 45.71679706732590631 ) ) ;
#8898 = CARTESIAN_POINT ( 'NONE',  ( -30.07540678000427548, 0.000000000000000000, 7.500000000000000000 ) ) ;
#8899 = VECTOR ( 'NONE', #4463, 1000.000000000000000 ) ;
#8900 = EDGE_LOOP ( 'NONE', ( #10775, #4039, #15802, #14089 ) ) ;
#8901 = CARTESIAN_POINT ( 'NONE',  ( 28.82574430125643516, -6.542305536751587880, 13.37088755551135932 ) ) ;
#8902 = DIRECTION ( 'NONE',  ( 0.000000000000000000, 1.000000000000000000, 0.000000000000000000 ) ) ;
#8903 = DIRECTION ( 'NONE',  ( 0.000000000000000000, 0.000000000000000000, 1.000000000000000000 ) ) ;
#8904 = VERTEX_POINT ( 'NONE', #15266 ) ;
#8905 = B_SPLINE_CURVE_WITH_KNOTS ( 'NONE', 3,
 ( #2864, #15935, #618, #12097, #20732, #3614, #18943, #8544, #7089, #13886 ),
 .UNSPECIFIED., .F., .F.,
 ( 4, 2, 2, 2, 4 ),
 ( 0.000000000000000000, 0.0001998921237118762633, 0.0003997842474237525267, 0.0007995684948475050534, 0.001599136989695010540 ),
 .UNSPECIFIED. ) ;
#8906 = ORIENTED_EDGE ( 'NONE', *, *, #15014, .F. ) ;
#8907 = CARTESIAN_POINT ( 'NONE',  ( 30.49999999999999645, 70.00000000000001421, 1.200000000000003064 ) ) ;
#8908 = CARTESIAN_POINT ( 'NONE',  ( -25.37540678000429395, -38.74634676501045760, 42.50000000000000000 ) ) ;
#8909 = CARTESIAN_POINT ( 'NONE',  ( -1.774728116533986544, 42.31054587065082728, 51.80876104995653719 ) ) ;
#8910 = EDGE_CURVE ( 'NONE', #21172, #15684, #10684, .T. ) ;
#8911 = DIRECTION ( 'NONE',  ( -0.000000000000000000, 1.000000000000000000, 0.000000000000000000 ) ) ;
#8912 = CIRCLE ( 'NONE', #2114, 0.2999999999999999334 ) ;
#8913 = ORIENTED_EDGE ( 'NONE', *, *, #18318, .T. ) ;
#8914 = DIRECTION ( 'NONE',  ( 0.000000000000000000, 0.000000000000000000, -1.000000000000000000 ) ) ;
#8915 = AXIS2_PLACEMENT_3D ( 'NONE', #19355, #429, #5388 ) ;
#8916 = VERTEX_POINT ( 'NONE', #20431 ) ;
#8917 = CARTESIAN_POINT ( 'NONE',  ( -15.95292532278785913, 52.39333383871510108, 13.79999999999999893 ) ) ;
#8918 = DIRECTION ( 'NONE',  ( -1.224646799147353207E-16, -0.000000000000000000, -1.000000000000000000 ) ) ;
#8919 = DIRECTION ( 'NONE',  ( 0.000000000000000000, 0.000000000000000000, 1.000000000000000000 ) ) ;
#8920 = DIRECTION ( 'NONE',  ( 0.000000000000000000, 0.000000000000000000, -1.000000000000000000 ) ) ;
#8921 = ORIENTED_EDGE ( 'NONE', *, *, #17425, .T. ) ;
#8922 = CYLINDRICAL_SURFACE ( 'NONE', #5943, 0.04999999999999991257 ) ;
#8923 = PLANE ( 'NONE',  #18904 ) ;
#8924 = CARTESIAN_POINT ( 'NONE',  ( 28.87540678000427619, 6.494748934539263274, 13.19999999999999929 ) ) ;
#8925 = DIRECTION ( 'NONE',  ( 1.000000000000000000, 0.000000000000000000, -0.000000000000000000 ) ) ;
#8926 = ORIENTED_EDGE ( 'NONE', *, *, #973, .T. ) ;
#8927 = ADVANCED_FACE ( 'NONE', ( #15149 ), #16722, .T. ) ;
#8929 = CIRCLE ( 'NONE', #17489, 4.193574995607837863 ) ;
#8928 = CARTESIAN_POINT ( 'NONE',  ( -30.37540678000427619, -6.000000000000000000, 7.200000000000000178 ) ) ;
#8930 = VERTEX_POINT ( 'NONE', #6675 ) ;
#8931 = AXIS2_PLACEMENT_3D ( 'NONE', #8041, #6260, #974 ) ;
#8932 = CIRCLE ( 'NONE', #1408, 0.2999999999999999334 ) ;
#8933 = CARTESIAN_POINT ( 'NONE',  ( -32.47706987357030073, 83.66206381164208494, 13.74999999999999822 ) ) ;
#8934 = CIRCLE ( 'NONE', #6814, 0.5000000000000004441 ) ;
#8935 = FACE_OUTER_BOUND ( 'NONE', #6341, .T. ) ;
#8936 = ORIENTED_EDGE ( 'NONE', *, *, #13166, .T. ) ;
#8937 = ORIENTED_EDGE ( 'NONE', *, *, #4308, .T. ) ;
#8938 = EDGE_CURVE ( 'NONE', #9117, #16813, #20315, .T. ) ;
#8939 = EDGE_CURVE ( 'NONE', #412, #9924, #18396, .T. ) ;
#8940 = LINE ( 'NONE', #414, #20675 ) ;
#8941 = ORIENTED_EDGE ( 'NONE', *, *, #13893, .F. ) ;
#8942 = VERTEX_POINT ( 'NONE', #1274 ) ;
#8943 = VECTOR ( 'NONE', #2189, 1000.000000000000000 ) ;
#8944 = AXIS2_PLACEMENT_3D ( 'NONE', #2082, #18997, #6930 ) ;
#8945 = ORIENTED_EDGE ( 'NONE', *, *, #3097, .T. ) ;
#8946 = CARTESIAN_POINT ( 'NONE',  ( -25.37540678000429040, -36.74634676501047181, 13.50000000000000000 ) ) ;
#8947 = PRESENTATION_LAYER_ASSIGNMENT (  '', '', ( #15719 ) ) ;
#8948 = DIRECTION ( 'NONE',  ( 0.000000000000000000, 1.000000000000000000, 0.000000000000000000 ) ) ;
#8949 = LINE ( 'NONE', #15528, #4935 ) ;
#8950 = EDGE_CURVE ( 'NONE', #18406, #3824, #5714, .T. ) ;
#8951 = CARTESIAN_POINT ( 'NONE',  ( 4.127054932750481520, -32.93424481021354921, 7.321391277662001151 ) ) ;
#8952 = ORIENTED_EDGE ( 'NONE', *, *, #11402, .T. ) ;
#8953 = LINE ( 'NONE', #21045, #12833 ) ;
#8954 = FACE_OUTER_BOUND ( 'NONE', #15875, .T. ) ;
#8955 = CARTESIAN_POINT ( 'NONE',  ( -31.31859531322107060, 84.19398174988410233, 68.50000000000000000 ) ) ;
#8956 = CIRCLE ( 'NONE', #11797, 0.3000000000000016542 ) ;
#8957 = EDGE_LOOP ( 'NONE', ( #13474, #4837, #18646, #16374 ) ) ;
#8958 = ADVANCED_FACE ( 'NONE', ( #21786 ), #18921, .T. ) ;
#8959 = CARTESIAN_POINT ( 'NONE',  ( 29.13662752439705272, 0.000000000000000000, 13.50000000000000000 ) ) ;
#8960 = AXIS2_PLACEMENT_3D ( 'NONE', #9997, #11651, #4962 ) ;
#8961 = VERTEX_POINT ( 'NONE', #21894 ) ;
#8962 = EDGE_CURVE ( 'NONE', #4728, #18442, #6571, .T. ) ;
#8963 = VERTEX_POINT ( 'NONE', #4873 ) ;
#8964 = ORIENTED_EDGE ( 'NONE', *, *, #17962, .F. ) ;
#8965 = CARTESIAN_POINT ( 'NONE',  ( -15.21174975910705207, -52.11873716947361856, 14.00000000000000000 ) ) ;
#8966 = EDGE_CURVE ( 'NONE', #4986, #5889, #1025, .T. ) ;
#8967 = SHAPE_DEFINITION_REPRESENTATION ( #18772, #9407 ) ;
#8968 = ORIENTED_EDGE ( 'NONE', *, *, #10134, .T. ) ;
#8969 = CARTESIAN_POINT ( 'NONE',  ( 23.02398829872513630, -2.681487294389184761, 13.50129116665758389 ) ) ;
#8970 = ORIENTED_EDGE ( 'NONE', *, *, #11921, .F. ) ;
#8971 = ORIENTED_EDGE ( 'NONE', *, *, #14020, .F. ) ;
#8972 = CARTESIAN_POINT ( 'NONE',  ( 15.21174975910707161, -52.11873716947361856, 68.00000000000000000 ) ) ;
#8973 = CARTESIAN_POINT ( 'NONE',  ( 14.71174975910707161, 51.61873716947361856, 68.00000000000000000 ) ) ;
#8974 = EDGE_CURVE ( 'NONE', #4820, #17759, #19992, .T. ) ;
#8975 = CARTESIAN_POINT ( 'NONE',  ( -29.13662752439705272, 0.000000000000000000, 1.500000000000001332 ) ) ;
#8976 = AXIS2_PLACEMENT_3D ( 'NONE', #19897, #12937, #1297 ) ;
#8977 =( NAMED_UNIT ( * ) PLANE_ANGLE_UNIT ( ) SI_UNIT ( $, .RADIAN. ) );
#8978 = CARTESIAN_POINT ( 'NONE',  ( -11.62890639357915923, 41.92645089659917801, 70.88527860057354246 ) ) ;
#8979 = DIRECTION ( 'NONE',  ( 1.000000000000000000, -0.000000000000000000, 6.123233995736764803E-17 ) ) ;
#8980 = DIRECTION ( 'NONE',  ( 0.000000000000000000, 0.000000000000000000, 1.000000000000000000 ) ) ;
#8981 = CYLINDRICAL_SURFACE ( 'NONE', #2130, 3.017785046117004377 ) ;
#8982 = TOROIDAL_SURFACE ( 'NONE', #7255, 1.000000000000000000, 0.5000000000000000000 ) ;
#8983 = CARTESIAN_POINT ( 'NONE',  ( -14.98825539710680488, -51.95771298364783775, 13.85621828746129225 ) ) ;
#8984 = AXIS2_PLACEMENT_3D ( 'NONE', #9781, #7773, #19740 ) ;
#8985 = EDGE_CURVE ( 'NONE', #9063, #7335, #20972, .T. ) ;
#8986 = ORIENTED_EDGE ( 'NONE', *, *, #17904, .F. ) ;
#8987 = VERTEX_POINT ( 'NONE', #17378 ) ;
#8988 = CARTESIAN_POINT ( 'NONE',  ( -9.141460742840918030, 32.93424481021354921, 68.50000000000000000 ) ) ;
#8989 = ADVANCED_FACE ( 'NONE', ( #18855 ), #3530, .T. ) ;
#8990 =( NAMED_UNIT ( * ) SI_UNIT ( $, .STERADIAN. ) SOLID_ANGLE_UNIT ( ) );
#8991 = DIRECTION ( 'NONE',  ( -1.788744114411106313E-17, -1.000000000000000000, -1.095289877103613968E-33 ) ) ;
#8992 = ORIENTED_EDGE ( 'NONE', *, *, #2405, .F. ) ;
#8993 = AXIS2_PLACEMENT_3D ( 'NONE', #3662, #5462, #15606 ) ;
#8994 = ORIENTED_EDGE ( 'NONE', *, *, #10465, .T. ) ;
#8995 = ORIENTED_EDGE ( 'NONE', *, *, #10693, .F. ) ;
#8996 = AXIS2_PLACEMENT_3D ( 'NONE', #10561, #9776, #16576 ) ;
#8997 = AXIS2_PLACEMENT_3D ( 'NONE', #5894, #13012, #19867 ) ;
#8998 = AXIS2_PLACEMENT_3D ( 'NONE', #18949, #11984, #133 ) ;
#8999 = PLANE ( 'NONE',  #3884 ) ;
#9000 = CIRCLE ( 'NONE', #1128, 0.05000000000000143219 ) ;
#9001 = CARTESIAN_POINT ( 'NONE',  ( -10.14415639357916099, 42.46645089659918426, 68.06527860057354928 ) ) ;
#9002 = ORIENTED_EDGE ( 'NONE', *, *, #10924, .F. ) ;
#9003 = CARTESIAN_POINT ( 'NONE',  ( 27.37540678000427619, 7.754037881813018962E-15, 42.50000000000000000 ) ) ;
#9004 = ADVANCED_FACE ( 'NONE', ( #5540 ), #2050, .T. ) ;
#9005 = CARTESIAN_POINT ( 'NONE',  ( 8.641460742840918030, -32.93424481021354921, 68.50000000000000000 ) ) ;
#9006 = DIRECTION ( 'NONE',  ( -0.000000000000000000, 0.000000000000000000, 1.000000000000000000 ) ) ;
#9007 = CARTESIAN_POINT ( 'NONE',  ( -14.75141514895149442, 52.14252005765843734, 13.49999999999999822 ) ) ;
#9008 = DIRECTION ( 'NONE',  ( -0.000000000000000000, -0.000000000000000000, -1.000000000000000000 ) ) ;
#9009 = ORIENTED_EDGE ( 'NONE', *, *, #10798, .F. ) ;
#9010 = CARTESIAN_POINT ( 'NONE',  ( -27.67540678000428400, -10.94079601157914716, 13.50000000000000000 ) ) ;
#9011 = CARTESIAN_POINT ( 'NONE',  ( 1.824728116533979705, 43.26054587065083012, 37.66679706732590915 ) ) ;
#9012 = CARTESIAN_POINT ( 'NONE',  ( -25.37540678000427263, -67.24634676501045760, 7.799999999999999822 ) ) ;
#9013 = ORIENTED_EDGE ( 'NONE', *, *, #5033, .T. ) ;
#9014 = ORIENTED_EDGE ( 'NONE', *, *, #2620, .T. ) ;
#9015 = ORIENTED_EDGE ( 'NONE', *, *, #14502, .T. ) ;
#9016 = CARTESIAN_POINT ( 'NONE',  ( -1.774728116533986766, 43.31054587065082728, 41.66679706732590915 ) ) ;
#9017 = DIRECTION ( 'NONE',  ( -0.000000000000000000, -0.000000000000000000, 1.000000000000000000 ) ) ;
#9018 = EDGE_CURVE ( 'NONE', #97, #1945, #17268, .T. ) ;
#9019 = AXIS2_PLACEMENT_3D ( 'NONE', #9194, #10769, #16003 ) ;
#9020 = DIRECTION ( 'NONE',  ( -1.224646799147353207E-16, -0.000000000000000000, -1.000000000000000000 ) ) ;
#9021 = ORIENTED_EDGE ( 'NONE', *, *, #4982, .T. ) ;
#9022 = PLANE ( 'NONE',  #16332 ) ;
#9023 = ORIENTED_EDGE ( 'NONE', *, *, #15004, .F. ) ;
#9024 = DIRECTION ( 'NONE',  ( 1.224646799147353207E-16, 0.000000000000000000, 1.000000000000000000 ) ) ;
#9025 = CARTESIAN_POINT ( 'NONE',  ( -30.19999999999999574, 70.00000000000000000, 1.199999999999999512 ) ) ;
#9026 = ORIENTED_EDGE ( 'NONE', *, *, #16477, .F. ) ;
#9027 = CARTESIAN_POINT ( 'NONE',  ( 1.824728116533979705, 43.31054587065082728, 29.66679706732590560 ) ) ;
#9028 = CARTESIAN_POINT ( 'NONE',  ( 17.45292532278785913, 38.74634676501045760, 14.00000000000000000 ) ) ;
#9029 = DIRECTION ( 'NONE',  ( -0.000000000000000000, 1.000000000000000000, -0.000000000000000000 ) ) ;
#9030 = CARTESIAN_POINT ( 'NONE',  ( 31.44597781366222122, 27.99124249474150972, 70.50000000000000000 ) ) ;
#9031 = EDGE_LOOP ( 'NONE', ( #8642, #1206, #21966, #9145 ) ) ;
#9032 = DIRECTION ( 'NONE',  ( -0.000000000000000000, -0.000000000000000000, -1.000000000000000000 ) ) ;
#9033 = DIRECTION ( 'NONE',  ( 0.000000000000000000, 0.000000000000000000, -1.000000000000000000 ) ) ;
#9034 = ADVANCED_FACE ( 'NONE', ( #7003 ), #20538, .T. ) ;
#9035 = CARTESIAN_POINT ( 'NONE',  ( 23.32398829872514057, -3.528912754968634768, 13.79999999999999893 ) ) ;
#9036 = DIRECTION ( 'NONE',  ( -1.000000000000000000, 0.000000000000000000, 0.000000000000000000 ) ) ;
#9037 = EDGE_LOOP ( 'NONE', ( #19975, #10609, #5395, #19108 ) ) ;
#9038 = EDGE_CURVE ( 'NONE', #5864, #17139, #21416, .T. ) ;
#9039 = CARTESIAN_POINT ( 'NONE',  ( 3.627054932750481964, -32.61873716947361856, 42.50000000000000000 ) ) ;
#9040 = EDGE_LOOP ( 'NONE', ( #5103, #665, #1224, #13743 ) ) ;
#9041 = DIRECTION ( 'NONE',  ( -1.000000000000000000, 0.000000000000000000, -6.123233995736764803E-17 ) ) ;
#9042 = DIRECTION ( 'NONE',  ( -0.000000000000000000, -1.000000000000000000, -0.000000000000000000 ) ) ;
#9043 = VERTEX_POINT ( 'NONE', #10682 ) ;
#9044 = EDGE_LOOP ( 'NONE', ( #11330, #2694, #7251, #6528 ) ) ;
#9045 = AXIS2_PLACEMENT_3D ( 'NONE', #9885, #16365, #21541 ) ;
#9046 = DIRECTION ( 'NONE',  ( 0.000000000000000000, 0.000000000000000000, 1.000000000000000000 ) ) ;
#9047 = CYLINDRICAL_SURFACE ( 'NONE', #2056, 5.000000000000000888 ) ;
#9048 = ORIENTED_EDGE ( 'NONE', *, *, #6572, .F. ) ;
#9049 = VERTEX_POINT ( 'NONE', #5660 ) ;
#9050 = ADVANCED_FACE ( 'NONE', ( #8574 ), #5207, .T. ) ;
#9051 = DIRECTION ( 'NONE',  ( 1.000000000000000000, 0.000000000000000000, 0.000000000000000000 ) ) ;
#9052 = CARTESIAN_POINT ( 'NONE',  ( -1.774728116533986766, 43.31054587065082728, 41.66679706732590915 ) ) ;
#9053 = CYLINDRICAL_SURFACE ( 'NONE', #16866, 0.5000000000000004441 ) ;
#9054 = DIRECTION ( 'NONE',  ( 1.000000000000000000, 0.000000000000000000, 0.000000000000000000 ) ) ;
#9055 = EDGE_CURVE ( 'NONE', #1152, #13238, #3552, .T. ) ;
#9056 = CARTESIAN_POINT ( 'NONE',  ( -22.16013893094044462, 45.60883947780118319, 68.50000000000000000 ) ) ;
#9057 = ORIENTED_EDGE ( 'NONE', *, *, #15335, .F. ) ;
#9058 = FACE_OUTER_BOUND ( 'NONE', #16197, .T. ) ;
#9059 = DIRECTION ( 'NONE',  ( 0.000000000000000000, 0.000000000000000000, 1.000000000000000000 ) ) ;
#9060 = FACE_BOUND ( 'NONE', #20992, .T. ) ;
#9061 = ORIENTED_EDGE ( 'NONE', *, *, #10429, .F. ) ;
#9062 = DIRECTION ( 'NONE',  ( -2.388292521039847891E-16, 0.000000000000000000, -1.000000000000000000 ) ) ;
#9063 = VERTEX_POINT ( 'NONE', #20651 ) ;
#9064 = ORIENTED_EDGE ( 'NONE', *, *, #21659, .F. ) ;
#9065 = LINE ( 'NONE', #15984, #6760 ) ;
#9066 = APPLICATION_PROTOCOL_DEFINITION ( 'draft international standard', 'automotive_design', 1998, #10013 ) ;
#9067 = ADVANCED_FACE ( 'NONE', ( #55 ), #15805, .F. ) ;
#9068 = ORIENTED_EDGE ( 'NONE', *, *, #12315, .F. ) ;
#9069 = VERTEX_POINT ( 'NONE', #6905 ) ;
#9070 = CARTESIAN_POINT ( 'NONE',  ( 17.95292532278785913, 34.11873716947361856, 13.49999999999999822 ) ) ;
#9071 = EDGE_LOOP ( 'NONE', ( #1605, #18149, #17747, #9064, #2316 ) ) ;
#9072 = CARTESIAN_POINT ( 'NONE',  ( -15.21174975910705207, 51.61873716947361856, 68.50000000000000000 ) ) ;
#9073 = ORIENTED_EDGE ( 'NONE', *, *, #7716, .F. ) ;
#9074 = EDGE_CURVE ( 'NONE', #1897, #8405, #9265, .T. ) ;
#9075 = CARTESIAN_POINT ( 'NONE',  ( 1.724728116533979616, 43.31054587065082728, 35.70876104995653577 ) ) ;
#9076 = EDGE_CURVE ( 'NONE', #21509, #12543, #16023, .T. ) ;
#9077 = CARTESIAN_POINT ( 'NONE',  ( -4.127054932750482408, 33.43424481021354921, 68.00000000000000000 ) ) ;
#9078 = VECTOR ( 'NONE', #16399, 1000.000000000000000 ) ;
#9079 = SURFACE_STYLE_USAGE ( .BOTH. , #5517 ) ;
#9080 = DIRECTION ( 'NONE',  ( 1.000000000000000000, 0.000000000000000000, 0.000000000000000000 ) ) ;
#9081 = ADVANCED_FACE ( 'NONE', ( #10241 ), #2164, .T. ) ;
#9082 = DIRECTION ( 'NONE',  ( -1.000000000000000000, 0.000000000000000000, 0.000000000000000000 ) ) ;
#9083 = CARTESIAN_POINT ( 'NONE',  ( 28.82574430125643516, 6.542305536751587880, 13.37088755551135932 ) ) ;
#9084 = CIRCLE ( 'NONE', #21956, 0.2999999999999999334 ) ;
#9085 = DIRECTION ( 'NONE',  ( 1.000000000000000000, 0.000000000000000000, 0.000000000000000000 ) ) ;
#9086 = LINE ( 'NONE', #2254, #14094 ) ;
#9087 = FACE_BOUND ( 'NONE', #863, .T. ) ;
#9088 = ORIENTED_EDGE ( 'NONE', *, *, #12070, .T. ) ;
#9089 = CARTESIAN_POINT ( 'NONE',  ( -28.57540678000427548, 6.776800961815481195, 13.50000000000000000 ) ) ;
#9090 = FILL_AREA_STYLE_COLOUR ( '', #10853 ) ;
#9091 = LINE ( 'NONE', #5422, #13110 ) ;
#9092 = ADVANCED_FACE ( 'NONE', ( #13689 ), #3640, .F. ) ;
#9093 = ORIENTED_EDGE ( 'NONE', *, *, #15850, .T. ) ;
#9094 = ORIENTED_EDGE ( 'NONE', *, *, #13987, .F. ) ;
#9095 = VECTOR ( 'NONE', #19276, 1000.000000000000000 ) ;
#9096 = EDGE_CURVE ( 'NONE', #20665, #1886, #14768, .T. ) ;
#9097 = FACE_OUTER_BOUND ( 'NONE', #5593, .T. ) ;
#9098 = EDGE_CURVE ( 'NONE', #16245, #13276, #21514, .T. ) ;
#9099 = CARTESIAN_POINT ( 'NONE',  ( -15.95292532278785913, -52.39333383871510108, 13.50000000000000000 ) ) ;
#9100 = ORIENTED_EDGE ( 'NONE', *, *, #19919, .F. ) ;
#9101 = DIRECTION ( 'NONE',  ( -0.9729678061520345977, -0.2309407893631976461, 0.000000000000000000 ) ) ;
#9102 = EDGE_CURVE ( 'NONE', #15132, #14744, #9985, .T. ) ;
#9103 = DIRECTION ( 'NONE',  ( -1.000000000000000000, 0.000000000000000000, -0.000000000000000000 ) ) ;
#9104 = DIRECTION ( 'NONE',  ( 1.000000000000000000, 0.000000000000000000, 0.000000000000000000 ) ) ;
#9105 = DIRECTION ( 'NONE',  ( 0.000000000000000000, 0.000000000000000000, 1.000000000000000000 ) ) ;
#9106 = CARTESIAN_POINT ( 'NONE',  ( 31.50000000000002132, 72.00000000000001421, 1.800000000000000044 ) ) ;
#9107 = CARTESIAN_POINT ( 'NONE',  ( 14.96174975910707161, 42.31054587065082728, 68.25000000000000000 ) ) ;
#9108 = DIRECTION ( 'NONE',  ( 0.000000000000000000, 0.000000000000000000, -1.000000000000000000 ) ) ;
#9109 = DIRECTION ( 'NONE',  ( -1.000000000000000000, 0.000000000000000000, 0.000000000000000000 ) ) ;
#9110 = DIRECTION ( 'NONE',  ( -0.000000000000000000, -0.000000000000000000, -1.000000000000000000 ) ) ;
#9111 = ORIENTED_EDGE ( 'NONE', *, *, #21821, .F. ) ;
#9112 = TOROIDAL_SURFACE ( 'NONE', #5915, 0.05000000000000000278, 0.05000000000000000278 ) ;
#9113 = ORIENTED_EDGE ( 'NONE', *, *, #6329, .F. ) ;
#9114 = CARTESIAN_POINT ( 'NONE',  ( 25.37540678000427263, 63.74634676501045050, 3.500000000000000000 ) ) ;
#9115 = DIRECTION ( 'NONE',  ( 0.000000000000000000, 0.000000000000000000, 1.000000000000000000 ) ) ;
#9116 = ADVANCED_FACE ( 'NONE', ( #7861 ), #1217, .T. ) ;
#9117 = VERTEX_POINT ( 'NONE', #585 ) ;
#9118 = LINE ( 'NONE', #12461, #11343 ) ;
#9119 = ADVANCED_FACE ( 'NONE', ( #12553 ), #17703, .T. ) ;
#9120 = ORIENTED_EDGE ( 'NONE', *, *, #17066, .T. ) ;
#9121 = CARTESIAN_POINT ( 'NONE',  ( 30.19999999999999574, 70.00000000000000000, 0.3000000000000033751 ) ) ;
#9122 = AXIS2_PLACEMENT_3D ( 'NONE', #7613, #6267, #14405 ) ;
#9123 = CARTESIAN_POINT ( 'NONE',  ( 0.000000000000000000, 68.74634676501045760, 7.500000000000000000 ) ) ;
#9124 = ORIENTED_EDGE ( 'NONE', *, *, #15850, .F. ) ;
#9125 = CARTESIAN_POINT ( 'NONE',  ( -29.13662752439705272, 0.000000000000000000, 0.3000000000000016542 ) ) ;
#9126 = CARTESIAN_POINT ( 'NONE',  ( 0.000000000000000000, -52.11873716947361856, 68.00000000000000000 ) ) ;
#9127 = AXIS2_PLACEMENT_3D ( 'NONE', #7333, #10894, #12560 ) ;
#9128 = DIRECTION ( 'NONE',  ( -0.000000000000000000, -0.000000000000000000, -1.000000000000000000 ) ) ;
#9129 = AXIS2_PLACEMENT_3D ( 'NONE', #15271, #20002, #6800 ) ;
#9130 = DIRECTION ( 'NONE',  ( -1.000000000000000000, -0.000000000000000000, -0.000000000000000000 ) ) ;
#9131 = AXIS2_PLACEMENT_3D ( 'NONE', #11235, #18059, #21666 ) ;
#9132 = VERTEX_POINT ( 'NONE', #18242 ) ;
#9133 = FACE_OUTER_BOUND ( 'NONE', #3391, .T. ) ;
#9134 = EDGE_CURVE ( 'NONE', #19220, #8405, #16776, .T. ) ;
#9135 = CARTESIAN_POINT ( 'NONE',  ( 15.21174975910707161, -52.11873716947361856, 68.00000000000000000 ) ) ;
#9136 = CARTESIAN_POINT ( 'NONE',  ( -21.92816239687475743, 42.46645089659918426, 13.74999999999999822 ) ) ;
#9137 = CARTESIAN_POINT ( 'NONE',  ( -23.05525514579169410, -2.329474921856953706, 13.28656140283153952 ) ) ;
#9138 = ORIENTED_EDGE ( 'NONE', *, *, #4293, .F. ) ;
#9139 = CARTESIAN_POINT ( 'NONE',  ( -15.21174975910705207, 52.39333383871510108, 13.50000000000000000 ) ) ;
#9140 = CARTESIAN_POINT ( 'NONE',  ( 14.96174975910705918, -32.10873716947361345, 13.79999999999999893 ) ) ;
#9141 = PLANE ( 'NONE',  #19518 ) ;
#9142 = SHAPE_REPRESENTATION ( 'Flap', ( #17493 ), #18569 ) ;
#9143 = VERTEX_POINT ( 'NONE', #19817 ) ;
#9144 = VECTOR ( 'NONE', #7297, 1000.000000000000000 ) ;
#9145 = ORIENTED_EDGE ( 'NONE', *, *, #7308, .T. ) ;
#9146 = DIRECTION ( 'NONE',  ( 1.000000000000000000, 0.000000000000000000, 0.000000000000000000 ) ) ;
#9147 = DIRECTION ( 'NONE',  ( 0.000000000000000000, 0.000000000000000000, 1.000000000000000000 ) ) ;
#9148 = ORIENTED_EDGE ( 'NONE', *, *, #16153, .F. ) ;
#9149 = AXIS2_PLACEMENT_3D ( 'NONE', #7445, #12995, #14250 ) ;
#9150 = TOROIDAL_SURFACE ( 'NONE', #11289, 1.000000000000000000, 0.5000000000000000000 ) ;
#9151 = EDGE_CURVE ( 'NONE', #2099, #1177, #10886, .T. ) ;
#9152 = EDGE_CURVE ( 'NONE', #8329, #7598, #16549, .T. ) ;
#9153 = ORIENTED_EDGE ( 'NONE', *, *, #22146, .T. ) ;
#9154 = EDGE_CURVE ( 'NONE', #5908, #1345, #11411, .T. ) ;
#9155 = APPLICATION_CONTEXT ( 'automotive_design' ) ;
#9156 = ORIENTED_EDGE ( 'NONE', *, *, #20512, .F. ) ;
#9157 = LINE ( 'NONE', #858, #19571 ) ;
#9158 = CIRCLE ( 'NONE', #4521, 0.05000000000000143219 ) ;
#9159 = AXIS2_PLACEMENT_3D ( 'NONE', #17948, #4646, #9788 ) ;
#9160 = AXIS2_PLACEMENT_3D ( 'NONE', #2897, #7939, #21591 ) ;
#9161 = LINE ( 'NONE', #17983, #7604 ) ;
#9162 = CARTESIAN_POINT ( 'NONE',  ( 1.774728116533979438, 42.31054587065082728, 27.80876104995653719 ) ) ;
#9163 = CARTESIAN_POINT ( 'NONE',  ( -9.718906393579157310, 40.01645089659919563, 70.88527860057354246 ) ) ;
#9164 = ORIENTED_EDGE ( 'NONE', *, *, #11363, .F. ) ;
#9165 = CARTESIAN_POINT ( 'NONE',  ( 14.66174975910705847, 51.76873716947361714, 13.50000000000000000 ) ) ;
#9166 = AXIS2_PLACEMENT_3D ( 'NONE', #10127, #6568, #22117 ) ;
#9167 = DIRECTION ( 'NONE',  ( 0.000000000000000000, -1.000000000000000000, 0.000000000000000000 ) ) ;
#9168 = EDGE_CURVE ( 'NONE', #14279, #13526, #10413, .T. ) ;
#9169 = ORIENTED_EDGE ( 'NONE', *, *, #22079, .F. ) ;
#9170 = DIRECTION ( 'NONE',  ( 0.000000000000000000, 1.000000000000000000, 0.000000000000000000 ) ) ;
#9171 = ORIENTED_EDGE ( 'NONE', *, *, #6871, .T. ) ;
#9172 = CIRCLE ( 'NONE', #18089, 0.04999999999999991257 ) ;
#9173 = VECTOR ( 'NONE', #10462, 1000.000000000000000 ) ;
#9174 = ORIENTED_EDGE ( 'NONE', *, *, #13350, .T. ) ;
#9175 = VECTOR ( 'NONE', #14546, 1000.000000000000000 ) ;
#9176 = DIRECTION ( 'NONE',  ( 1.000000000000000000, 0.000000000000000000, 0.000000000000000000 ) ) ;
#9177 = EDGE_CURVE ( 'NONE', #11406, #8743, #14873, .T. ) ;
#9178 = ORIENTED_EDGE ( 'NONE', *, *, #16988, .T. ) ;
#9179 = ORIENTED_EDGE ( 'NONE', *, *, #10478, .T. ) ;
#9180 = EDGE_CURVE ( 'NONE', #170, #7349, #4261, .T. ) ;
#9181 = AXIS2_PLACEMENT_3D ( 'NONE', #11861, #5057, #18695 ) ;
#9182 = CARTESIAN_POINT ( 'NONE',  ( -1.724728116533986721, 42.31054587065082728, 31.80876104995653719 ) ) ;
#9183 = VERTEX_POINT ( 'NONE', #3973 ) ;
#9184 = CYLINDRICAL_SURFACE ( 'NONE', #2893, 0.3000000000000016542 ) ;
#9185 = CARTESIAN_POINT ( 'NONE',  ( 0.000000000000000000, 52.39333383871510108, 13.79999999999999893 ) ) ;
#9186 = CARTESIAN_POINT ( 'NONE',  ( 34.99999999999999289, 84.70000000000001705, 80.00000000000000000 ) ) ;
#9187 = DIRECTION ( 'NONE',  ( 0.000000000000000000, 0.000000000000000000, -1.000000000000000000 ) ) ;
#9188 = VECTOR ( 'NONE', #4288, 1000.000000000000000 ) ;
#9189 = VECTOR ( 'NONE', #11945, 1000.000000000000000 ) ;
#9190 = AXIS2_PLACEMENT_3D ( 'NONE', #18927, #8635, #13547 ) ;
#9191 = PLANE ( 'NONE',  #20051 ) ;
#9192 = CARTESIAN_POINT ( 'NONE',  ( 28.87540678000427619, 6.494748934539263274, 13.19999999999999929 ) ) ;
#9193 = AXIS2_PLACEMENT_3D ( 'NONE', #16817, #18382, #1715 ) ;
#9194 = CARTESIAN_POINT ( 'NONE',  ( 0.000000000000000000, 43.31054587065082728, 12.00000000000000000 ) ) ;
#9196 = EDGE_CURVE ( 'NONE', #13259, #15133, #6438, .T. ) ;
#9195 = DIRECTION ( 'NONE',  ( -2.546383084002652634E-16, -0.000000000000000000, -1.000000000000000000 ) ) ;
#9197 = DIRECTION ( 'NONE',  ( 0.000000000000000000, 0.000000000000000000, 1.000000000000000000 ) ) ;
#9198 = AXIS2_PLACEMENT_3D ( 'NONE', #13868, #213, #3813 ) ;
#9199 = EDGE_LOOP ( 'NONE', ( #19335, #1470, #20924, #9679, #16097, #16821, #86, #20833 ) ) ;
#9200 = CARTESIAN_POINT ( 'NONE',  ( 17.93704824106378837, 38.74634676501045760, 13.87500000000000000 ) ) ;
#9201 = EDGE_CURVE ( 'NONE', #15111, #13985, #6184, .T. ) ;
#9202 = ORIENTED_EDGE ( 'NONE', *, *, #11546, .F. ) ;
#9203 = AXIS2_PLACEMENT_3D ( 'NONE', #11259, #7936, #2994 ) ;
#9204 = AXIS2_PLACEMENT_3D ( 'NONE', #2446, #14071, #12385 ) ;
#9205 = AXIS2_PLACEMENT_3D ( 'NONE', #19802, #3010, #9737 ) ;
#9206 = ORIENTED_EDGE ( 'NONE', *, *, #12315, .T. ) ;
#9207 = TOROIDAL_SURFACE ( 'NONE', #5303, 0.5999999999999999778, 0.2999999999999999889 ) ;
#9208 = TOROIDAL_SURFACE ( 'NONE', #12061, 0.5999999999999999778, 0.2999999999999999889 ) ;
#9209 = CIRCLE ( 'NONE', #4923, 0.3000000000000016542 ) ;
#9210 = CARTESIAN_POINT ( 'NONE',  ( -15.21174975910705207, 51.86873716947361856, 13.05380965755523448 ) ) ;
#9211 = CARTESIAN_POINT ( 'NONE',  ( 0.000000000000000000, 38.74634676501045760, 42.50000000000000000 ) ) ;
#9212 = ORIENTED_EDGE ( 'NONE', *, *, #18939, .F. ) ;
#9213 = DIRECTION ( 'NONE',  ( 1.000000000000000000, -0.000000000000000000, 6.123233995736764803E-17 ) ) ;
#9214 = CARTESIAN_POINT ( 'NONE',  ( 23.05525514579170121, 2.329474921856955039, 13.28656140283153420 ) ) ;
#9215 = EDGE_CURVE ( 'NONE', #19777, #961, #21079, .T. ) ;
#9216 = CARTESIAN_POINT ( 'NONE',  ( -1.724728116533986721, 43.26054587065083012, 29.76679706732590702 ) ) ;
#9217 = DIRECTION ( 'NONE',  ( 1.000000000000000000, 0.000000000000000000, 0.000000000000000000 ) ) ;
#9218 = DIRECTION ( 'NONE',  ( 0.000000000000000000, 1.000000000000000000, 0.000000000000000000 ) ) ;
#9219 = CIRCLE ( 'NONE', #9951, 1.499999999999999556 ) ;
#9220 = AXIS2_PLACEMENT_3D ( 'NONE', #1654, #20241, #8497 ) ;
#9221 = CARTESIAN_POINT ( 'NONE',  ( -23.02398829872513986, 3.528912754968630328, 13.79999999999999893 ) ) ;
#9222 = EDGE_LOOP ( 'NONE', ( #10073, #4408, #4386, #7772 ) ) ;
#9223 = DIRECTION ( 'NONE',  ( 0.000000000000000000, -1.000000000000000000, 0.000000000000000000 ) ) ;
#9224 = CARTESIAN_POINT ( 'NONE',  ( -1.724728116533986721, 43.26054587065083012, 35.75876104995654003 ) ) ;
#9225 = CIRCLE ( 'NONE', #14563, 0.2999999999999947153 ) ;
#9226 = DIRECTION ( 'NONE',  ( 0.000000000000000000, 0.000000000000000000, 1.000000000000000000 ) ) ;
#9227 = ORIENTED_EDGE ( 'NONE', *, *, #1242, .T. ) ;
#9228 = VERTEX_POINT ( 'NONE', #16449 ) ;
#9229 = TOROIDAL_SURFACE ( 'NONE', #21032, 0.2500000000000000000, 0.2500000000000000000 ) ;
#9230 = ORIENTED_EDGE ( 'NONE', *, *, #805, .T. ) ;
#9231 = DIRECTION ( 'NONE',  ( -0.000000000000000000, -0.000000000000000000, -1.000000000000000000 ) ) ;
#9232 = AXIS2_PLACEMENT_3D ( 'NONE', #2870, #3764, #8807 ) ;
#9233 = CARTESIAN_POINT ( 'NONE',  ( -21.71259690522456154, 45.22582864897715638, 68.25000000000000000 ) ) ;
#9234 = EDGE_CURVE ( 'NONE', #16676, #15319, #13739, .T. ) ;
#9235 = EDGE_LOOP ( 'NONE', ( #10372, #5175, #6777, #1430 ) ) ;
#9236 = EDGE_CURVE ( 'NONE', #879, #21684, #18796, .T. ) ;
#9237 = DIRECTION ( 'NONE',  ( -1.000000000000000000, 0.000000000000000000, 0.000000000000000000 ) ) ;
#9238 = ADVANCED_FACE ( 'NONE', ( #4932 ), #339, .T. ) ;
#9239 = EDGE_LOOP ( 'NONE', ( #14112, #6430, #6301, #20462 ) ) ;
#9240 = DIRECTION ( 'NONE',  ( 1.000000000000000000, 0.000000000000000000, 0.000000000000000000 ) ) ;
#9241 = CIRCLE ( 'NONE', #16741, 3.017785046117004377 ) ;
#9242 = DIRECTION ( 'NONE',  ( 1.000000000000000000, 0.000000000000000000, 0.000000000000000000 ) ) ;
#9243 = CARTESIAN_POINT ( 'NONE',  ( -29.50000000000002132, 69.00000000000000000, -150.0833101980363722 ) ) ;
#9244 = LINE ( 'NONE', #7674, #295 ) ;
#9245 = VECTOR ( 'NONE', #22030, 1000.000000000000114 ) ;
#9246 = VECTOR ( 'NONE', #11996, 1000.000000000000000 ) ;
#9247 = CARTESIAN_POINT ( 'NONE',  ( 27.37540678000427974, -5.683640910026986681, 42.50000000000000000 ) ) ;
#9248 = FACE_OUTER_BOUND ( 'NONE', #19168, .T. ) ;
#9249 = ORIENTED_EDGE ( 'NONE', *, *, #20063, .F. ) ;
#9250 = DIRECTION ( 'NONE',  ( 0.000000000000000000, -1.000000000000000000, 0.000000000000000000 ) ) ;
#9251 = EDGE_CURVE ( 'NONE', #20337, #9771, #5724, .T. ) ;
#9252 = DIRECTION ( 'NONE',  ( -6.375533427066372209E-18, 0.4461977533474357216, -0.8949343913984425525 ) ) ;
#9253 = CARTESIAN_POINT ( 'NONE',  ( 1.824728116533979261, 43.31054587065082728, 47.80876104995653719 ) ) ;
#9254 = ORIENTED_EDGE ( 'NONE', *, *, #2853, .F. ) ;
#9255 = DIRECTION ( 'NONE',  ( 0.000000000000000000, 0.000000000000000000, -1.000000000000000000 ) ) ;
#9256 = ORIENTED_EDGE ( 'NONE', *, *, #16069, .F. ) ;
#9257 = DIRECTION ( 'NONE',  ( 0.000000000000000000, 0.000000000000000000, 1.000000000000000000 ) ) ;
#9259 = AXIS2_PLACEMENT_3D ( 'NONE', #10130, #3641, #17269 ) ;
#9258 = CARTESIAN_POINT ( 'NONE',  ( -15.21174975910705207, 52.11873716947361856, 14.00000000000000000 ) ) ;
#9260 = ORIENTED_EDGE ( 'NONE', *, *, #9520, .T. ) ;
#9261 = ORIENTED_EDGE ( 'NONE', *, *, #20465, .T. ) ;
#9262 = CARTESIAN_POINT ( 'NONE',  ( 17.93704824106378837, 50.11873716947361856, 13.87499999999999822 ) ) ;
#9263 = DIRECTION ( 'NONE',  ( 0.000000000000000000, 0.000000000000000000, -1.000000000000000000 ) ) ;
#9264 = DIRECTION ( 'NONE',  ( 0.000000000000000000, 1.000000000000000000, 0.000000000000000000 ) ) ;
#9265 = CIRCLE ( 'NONE', #11743, 0.05000000000000143219 ) ;
#9266 = EDGE_CURVE ( 'NONE', #20894, #6809, #6790, .T. ) ;
#9267 = VERTEX_POINT ( 'NONE', #5271 ) ;
#9268 = ADVANCED_FACE ( 'NONE', ( #16995 ), #20379, .T. ) ;
#9269 = AXIS2_PLACEMENT_3D ( 'NONE', #5272, #2000, #19129 ) ;
#9270 = ORIENTED_EDGE ( 'NONE', *, *, #5557, .T. ) ;
#9271 = VERTEX_POINT ( 'NONE', #12069 ) ;
#9272 = CYLINDRICAL_SURFACE ( 'NONE', #17775, 0.05000000000000143219 ) ;
#9273 = DIRECTION ( 'NONE',  ( 0.000000000000000000, 0.000000000000000000, 1.000000000000000000 ) ) ;
#9274 = DIRECTION ( 'NONE',  ( 0.000000000000000000, -1.000000000000000000, 0.000000000000000000 ) ) ;
#9275 = DIRECTION ( 'NONE',  ( 0.000000000000000000, 1.000000000000000000, 0.000000000000000000 ) ) ;
#9276 = AXIS2_PLACEMENT_3D ( 'NONE', #5416, #12303, #8875 ) ;
#9277 = CIRCLE ( 'NONE', #6069, 1.000000000000000888 ) ;
#9278 = FACE_OUTER_BOUND ( 'NONE', #14148, .T. ) ;
#9279 = ORIENTED_EDGE ( 'NONE', *, *, #4365, .F. ) ;
#9280 = CARTESIAN_POINT ( 'NONE',  ( -17.92752199202934094, 38.74634676501045760, 13.79999999999999893 ) ) ;
#9281 = EDGE_CURVE ( 'NONE', #1657, #18203, #1038, .T. ) ;
#9282 = CARTESIAN_POINT ( 'NONE',  ( -1.724728116533986721, 43.31054587065082728, 41.66679706732590915 ) ) ;
#9283 = DIRECTION ( 'NONE',  ( -0.000000000000000000, 0.000000000000000000, 1.000000000000000000 ) ) ;
#9284 = DIRECTION ( 'NONE',  ( 0.000000000000000000, 0.000000000000000000, -1.000000000000000000 ) ) ;
#9285 = ORIENTED_EDGE ( 'NONE', *, *, #19954, .T. ) ;
#9286 = DIRECTION ( 'NONE',  ( -0.000000000000000000, 1.000000000000000000, 0.000000000000000000 ) ) ;
#9287 = ORIENTED_EDGE ( 'NONE', *, *, #328, .F. ) ;
#9288 = VERTEX_POINT ( 'NONE', #13646 ) ;
#9289 = DIRECTION ( 'NONE',  ( 1.000000000000000000, -0.000000000000000000, -0.000000000000000000 ) ) ;
#9291 = EDGE_CURVE ( 'NONE', #7172, #14913, #16893, .T. ) ;
#9290 = ITEM_DEFINED_TRANSFORMATION ( 'NONE', 'NONE', #20158,  #17493 ) ;
#9292 = B_SPLINE_CURVE_WITH_KNOTS ( 'NONE', 3,
 ( #13859, #15970, #20708, #12278, #17324, #1996, #19127, #428 ),
 .UNSPECIFIED., .F., .F.,
 ( 4, 2, 2, 4 ),
 ( 0.000000000000000000, 0.0001479575850294295161, 0.0002959151700588590322, 0.0005918303401177112339 ),
 .UNSPECIFIED. ) ;
#9293 = ORIENTED_EDGE ( 'NONE', *, *, #5955, .T. ) ;
#9294 = VECTOR ( 'NONE', #2606, 1000.000000000000000 ) ;
#9295 = CIRCLE ( 'NONE', #8591, 0.05000000000000143219 ) ;
#9296 = VERTEX_POINT ( 'NONE', #205 ) ;
#9297 = DIRECTION ( 'NONE',  ( 0.000000000000000000, 1.000000000000000000, 0.000000000000000000 ) ) ;
#9298 = EDGE_LOOP ( 'NONE', ( #16319, #21133, #12445, #16013 ) ) ;
#9299 = LINE ( 'NONE', #9072, #9304 ) ;
#9300 = DIRECTION ( 'NONE',  ( 0.000000000000000000, -1.000000000000000000, 0.000000000000000000 ) ) ;
#9301 = CARTESIAN_POINT ( 'NONE',  ( 25.37540678000427263, 63.74634676501045050, 3.799999999999999822 ) ) ;
#9302 = CARTESIAN_POINT ( 'NONE',  ( -28.87540678000427619, -63.74634676501045050, 13.50000000000000000 ) ) ;
#9303 = CARTESIAN_POINT ( 'NONE',  ( -31.50000000000002132, 71.70000000000001705, 3.500000000000000000 ) ) ;
#9304 = VECTOR ( 'NONE', #18007, 1000.000000000000000 ) ;
#9305 = EDGE_CURVE ( 'NONE', #19733, #9618, #3591, .T. ) ;
#9306 = AXIS2_PLACEMENT_3D ( 'NONE', #17248, #10214, #1584 ) ;
#9307 = CARTESIAN_POINT ( 'NONE',  ( -1.724728116533986721, 43.31054587065082728, 39.75876104995654003 ) ) ;
#9308 = DIRECTION ( 'NONE',  ( -0.000000000000000000, 1.000000000000000000, -0.000000000000000000 ) ) ;
#9309 = EDGE_CURVE ( 'NONE', #16076, #21435, #8569, .T. ) ;
#9310 = CARTESIAN_POINT ( 'NONE',  ( -1.724728116533986721, 43.31054587065082728, 49.66679706732590915 ) ) ;
#9311 = DIRECTION ( 'NONE',  ( 1.000000000000000000, 0.000000000000000000, 0.000000000000000000 ) ) ;
#9312 = ORIENTED_EDGE ( 'NONE', *, *, #18683, .F. ) ;
#9313 = ORIENTED_EDGE ( 'NONE', *, *, #16871, .F. ) ;
#9314 = CARTESIAN_POINT ( 'NONE',  ( 23.02398829872514341, -5.683640910026986681, 13.79999999999999893 ) ) ;
#9315 = FILL_AREA_STYLE ('',( #9090 ) ) ;
#9316 = ORIENTED_EDGE ( 'NONE', *, *, #10937, .T. ) ;
#9317 = CIRCLE ( 'NONE', #21127, 0.5000000000000004441 ) ;
#9318 = VECTOR ( 'NONE', #11382, 1000.000000000000000 ) ;
#9319 = EDGE_CURVE ( 'NONE', #15347, #16035, #14992, .T. ) ;
#9320 = CARTESIAN_POINT ( 'NONE',  ( 14.75227361498200551, -52.14371094787964722, 13.50000000000000000 ) ) ;
#9321 = LINE ( 'NONE', #7650, #13434 ) ;
#9322 = ORIENTED_EDGE ( 'NONE', *, *, #5591, .T. ) ;
#9323 = FACE_BOUND ( 'NONE', #2292, .T. ) ;
#9324 = EDGE_CURVE ( 'NONE', #21509, #16219, #18456, .T. ) ;
#9325 = CARTESIAN_POINT ( 'NONE',  ( -32.50000000000002132, 72.00000000000001421, 1.800000000000000044 ) ) ;
#9326 = CIRCLE ( 'NONE', #2546, 1.000000000000000888 ) ;
#9327 = CARTESIAN_POINT ( 'NONE',  ( -28.79994065384636315, 6.566898051583388352, 13.40260211333369256 ) ) ;
#9328 = CARTESIAN_POINT ( 'NONE',  ( -23.08512718742728964, 2.485300415563057808, 13.35387015137020050 ) ) ;
#9329 = ORIENTED_EDGE ( 'NONE', *, *, #15109, .T. ) ;
#9330 = LINE ( 'NONE', #14028, #10774 ) ;
#9331 = CIRCLE ( 'NONE', #7557, 0.3000000000000004885 ) ;
#9332 = LINE ( 'NONE', #14692, #3072 ) ;
#9333 = DIRECTION ( 'NONE',  ( 1.000000000000000000, 0.000000000000000000, 0.000000000000000000 ) ) ;
#9334 = ORIENTED_EDGE ( 'NONE', *, *, #19141, .F. ) ;
#9335 = EDGE_LOOP ( 'NONE', ( #18787, #15895, #12473, #11338, #14355, #2984, #5651, #16283 ) ) ;
#9336 = VERTEX_POINT ( 'NONE', #1892 ) ;
#9337 = CARTESIAN_POINT ( 'NONE',  ( -23.02398829872513986, -2.157133568460768647, 13.19999999999999929 ) ) ;
#9338 = DIRECTION ( 'NONE',  ( 0.000000000000000000, 1.000000000000000000, 0.000000000000000000 ) ) ;
#9339 = ORIENTED_EDGE ( 'NONE', *, *, #21832, .T. ) ;
#9340 = AXIS2_PLACEMENT_3D ( 'NONE', #17704, #7223, #587 ) ;
#9341 = CYLINDRICAL_SURFACE ( 'NONE', #2363, 5.000000000000004441 ) ;
#9342 = EDGE_CURVE ( 'NONE', #4085, #18476, #9970, .T. ) ;
#9343 = VECTOR ( 'NONE', #11879, 1000.000000000000000 ) ;
#9344 = CIRCLE ( 'NONE', #4353, 0.05000000000000143219 ) ;
#9345 = ORIENTED_EDGE ( 'NONE', *, *, #1473, .T. ) ;
#9346 = DIRECTION ( 'NONE',  ( 0.000000000000000000, 0.000000000000000000, 1.000000000000000000 ) ) ;
#9347 = CARTESIAN_POINT ( 'NONE',  ( -9.641460742840918030, -32.61873716947361856, 68.00000000000000000 ) ) ;
#9348 = CARTESIAN_POINT ( 'NONE',  ( 1.724728116533979616, 42.36054587065083155, 49.76679706732591058 ) ) ;
#9349 = DIRECTION ( 'NONE',  ( 3.052134192567367925E-16, 1.000000000000000000, 0.000000000000000000 ) ) ;
#9350 = FACE_OUTER_BOUND ( 'NONE', #362, .T. ) ;
#9351 = DIRECTION ( 'NONE',  ( 0.000000000000000000, 0.000000000000000000, -1.000000000000000000 ) ) ;
#9352 = ORIENTED_EDGE ( 'NONE', *, *, #15368, .F. ) ;
#9353 = CARTESIAN_POINT ( 'NONE',  ( 17.45292532278785913, 0.000000000000000000, 14.00000000000000000 ) ) ;
#9354 = CARTESIAN_POINT ( 'NONE',  ( 25.37540678000427263, 66.94634676501046044, 13.19999999999999929 ) ) ;
#9355 = ADVANCED_FACE ( 'NONE', ( #8294 ), #11744, .T. ) ;
#9356 = EDGE_CURVE ( 'NONE', #15579, #6378, #8515, .T. ) ;
#9357 = ADVANCED_FACE ( 'NONE', ( #3252 ), #5156, .T. ) ;
#9358 = DIRECTION ( 'NONE',  ( 2.832483164223434527E-16, 1.000000000000000000, 0.000000000000000000 ) ) ;
#9359 = CARTESIAN_POINT ( 'NONE',  ( -23.08502376492393182, -2.484776121502528134, 13.35369709827396534 ) ) ;
#9360 = VERTEX_POINT ( 'NONE', #3470 ) ;
#9361 = AXIS2_PLACEMENT_3D ( 'NONE', #4533, #16392, #7473 ) ;
#9362 = FACE_OUTER_BOUND ( 'NONE', #20210, .T. ) ;
#9363 = AXIS2_PLACEMENT_3D ( 'NONE', #7534, #2359, #12203 ) ;
#9364 = VERTEX_POINT ( 'NONE', #10309 ) ;
#9365 = AXIS2_PLACEMENT_3D ( 'NONE', #21615, #4472, #4262 ) ;
#9366 = CARTESIAN_POINT ( 'NONE',  ( -1.724728116533986721, 43.26054587065083012, 43.75876104995654003 ) ) ;
#9367 = VECTOR ( 'NONE', #2658, 1000.000000000000000 ) ;
#9368 = ORIENTED_EDGE ( 'NONE', *, *, #9678, .T. ) ;
#9369 = AXIS2_PLACEMENT_3D ( 'NONE', #16544, #12626, #10466 ) ;
#9370 = EDGE_LOOP ( 'NONE', ( #13428, #13212, #8139, #3349 ) ) ;
#9371 = FACE_OUTER_BOUND ( 'NONE', #18310, .T. ) ;
#9372 = LINE ( 'NONE', #4557, #7788 ) ;
#9373 = CARTESIAN_POINT ( 'NONE',  ( 29.69597781366221767, 58.94165929845684104, 70.25000000000000000 ) ) ;
#9374 = ORIENTED_EDGE ( 'NONE', *, *, #21721, .T. ) ;
#9375 = ADVANCED_FACE ( 'NONE', ( #6957 ), #18935, .F. ) ;
#9376 = ORIENTED_EDGE ( 'NONE', *, *, #11946, .F. ) ;
#9377 = DIRECTION ( 'NONE',  ( -1.000000000000000000, 0.000000000000000000, 0.000000000000000000 ) ) ;
#9378 = AXIS2_PLACEMENT_3D ( 'NONE', #20823, #12177, #12509 ) ;
#9379 = ORIENTED_EDGE ( 'NONE', *, *, #19863, .T. ) ;
#9380 = CARTESIAN_POINT ( 'NONE',  ( 1.724728116533979838, 42.36054587065083155, 29.66679706732590560 ) ) ;
#9381 = AXIS2_PLACEMENT_3D ( 'NONE', #14353, #21099, #10890 ) ;
#9382 = DIRECTION ( 'NONE',  ( 0.000000000000000000, 0.000000000000000000, 1.000000000000000000 ) ) ;
#9383 = LINE ( 'NONE', #16184, #2947 ) ;
#9384 = CARTESIAN_POINT ( 'NONE',  ( -25.37540678000427263, -63.74634676501045050, 7.200000000000000178 ) ) ;
#9385 = EDGE_CURVE ( 'NONE', #13366, #14054, #20556, .T. ) ;
#9386 = EDGE_CURVE ( 'NONE', #5113, #818, #10703, .T. ) ;
#9387 = DIRECTION ( 'NONE',  ( 0.000000000000000000, -1.000000000000000000, 0.000000000000000000 ) ) ;
#9388 = ORIENTED_EDGE ( 'NONE', *, *, #1699, .F. ) ;
#9389 = DIRECTION ( 'NONE',  ( -0.000000000000000000, 0.000000000000000000, 1.000000000000000000 ) ) ;
#9390 = AXIS2_PLACEMENT_3D ( 'NONE', #11547, #6206, #12993 ) ;
#9391 = EDGE_CURVE ( 'NONE', #1947, #10547, #8953, .T. ) ;
#9392 = DIRECTION ( 'NONE',  ( -0.000000000000000000, -0.000000000000000000, 1.000000000000000000 ) ) ;
#9393 = DIRECTION ( 'NONE',  ( 0.000000000000000000, 0.000000000000000000, -1.000000000000000000 ) ) ;
#9394 = CARTESIAN_POINT ( 'NONE',  ( 1.774728116533979438, 42.31054587065082728, 51.80876104995653719 ) ) ;
#9395 = VERTEX_POINT ( 'NONE', #5727 ) ;
#9396 = ORIENTED_EDGE ( 'NONE', *, *, #921, .F. ) ;
#9397 = CARTESIAN_POINT ( 'NONE',  ( 26.63662752439704917, 3.061616997868386099E-16, -18.50000000000000000 ) ) ;
#9398 = CONTEXT_DEPENDENT_SHAPE_REPRESENTATION ( #5022, #15374 ) ;
#9399 = EDGE_CURVE ( 'NONE', #1748, #1165, #8912, .T. ) ;
#9400 = VERTEX_POINT ( 'NONE', #653 ) ;
#9401 = EDGE_LOOP ( 'NONE', ( #18042, #736, #738, #17134 ) ) ;
#9402 = CARTESIAN_POINT ( 'NONE',  ( -21.87350007617872905, 45.48374084210715296, 13.75000000000000000 ) ) ;
#9403 = ADVANCED_FACE ( 'NONE', ( #9058 ), #17447, .T. ) ;
#9404 = CARTESIAN_POINT ( 'NONE',  ( -9.178906393579158163, 42.46645089659918426, 70.38908280829822672 ) ) ;
#9405 = ORIENTED_EDGE ( 'NONE', *, *, #15632, .F. ) ;
#9406 = DIRECTION ( 'NONE',  ( 1.000000000000000000, 0.000000000000000000, 0.000000000000000000 ) ) ;
#9407 = SHAPE_REPRESENTATION ( 'Main Body', ( #17493 ), #10355 ) ;
#9408 = VERTEX_POINT ( 'NONE', #14304 ) ;
#9409 = CARTESIAN_POINT ( 'NONE',  ( -31.69597781366221412, 27.99124249474150972, 68.75000000000000000 ) ) ;
#9410 = FACE_OUTER_BOUND ( 'NONE', #2487, .T. ) ;
#9411 = DIRECTION ( 'NONE',  ( 0.000000000000000000, 0.000000000000000000, -1.000000000000000000 ) ) ;
#9412 = DIRECTION ( 'NONE',  ( 0.000000000000000000, -1.000000000000000000, 0.000000000000000000 ) ) ;
#9413 = EDGE_CURVE ( 'NONE', #17690, #6786, #20360, .T. ) ;
#9414 = CARTESIAN_POINT ( 'NONE',  ( -8.638906393579159015, 41.43704565779017202, 70.88527860057354246 ) ) ;
#9415 = CYLINDRICAL_SURFACE ( 'NONE', #10090, 0.04999999999999991257 ) ;
#9416 = FACE_OUTER_BOUND ( 'NONE', #6919, .T. ) ;
#9417 = FACE_BOUND ( 'NONE', #18882, .T. ) ;
#9418 = LINE ( 'NONE', #7744, #9175 ) ;
#9419 = CARTESIAN_POINT ( 'NONE',  ( -8.638906393579159015, 43.51045099701597252, 68.06527860057354928 ) ) ;
#9420 = CARTESIAN_POINT ( 'NONE',  ( -15.95292532278785913, -50.11873716947361856, 109.6002446535588319 ) ) ;
#9421 = VERTEX_POINT ( 'NONE', #7173 ) ;
#9422 = ORIENTED_EDGE ( 'NONE', *, *, #11828, .F. ) ;
#9423 = SURFACE_SIDE_STYLE ('',( #17917 ) ) ;
#9424 = CARTESIAN_POINT ( 'NONE',  ( 0.000000000000000000, 43.26054587065083012, 29.71679706732590631 ) ) ;
#9425 = VERTEX_POINT ( 'NONE', #14186 ) ;
#9426 = ORIENTED_EDGE ( 'NONE', *, *, #4167, .F. ) ;
#9427 = EDGE_CURVE ( 'NONE', #1527, #20601, #20724, .T. ) ;
#9428 = AXIS2_PLACEMENT_3D ( 'NONE', #19104, #4005, #10820 ) ;
#9429 = EDGE_CURVE ( 'NONE', #8585, #2941, #15859, .T. ) ;
#9430 = EDGE_CURVE ( 'NONE', #16243, #8345, #3571, .T. ) ;
#9431 = LINE ( 'NONE', #6309, #9188 ) ;
#9432 = AXIS2_PLACEMENT_3D ( 'NONE', #18130, #13315, #13648 ) ;
#9433 = CARTESIAN_POINT ( 'NONE',  ( -9.718906393579157310, 43.51045099701597962, 68.06527860057354928 ) ) ;
#9434 = ORIENTED_EDGE ( 'NONE', *, *, #15259, .T. ) ;
#9435 = DIRECTION ( 'NONE',  ( 1.000000000000000000, 0.000000000000000000, 0.000000000000000000 ) ) ;
#9436 = CARTESIAN_POINT ( 'NONE',  ( 14.66174975910705847, 51.76873716947361004, 13.50000000000000000 ) ) ;
#9437 = CARTESIAN_POINT ( 'NONE',  ( 1.774728116533979883, 42.36054587065083155, 45.66679706732590205 ) ) ;
#9438 = DIRECTION ( 'NONE',  ( 0.000000000000000000, -0.000000000000000000, -1.000000000000000000 ) ) ;
#9439 = ORIENTED_EDGE ( 'NONE', *, *, #4832, .T. ) ;
#9440 = CARTESIAN_POINT ( 'NONE',  ( 14.96174975910705918, 51.61873716947361856, 14.00000000000000000 ) ) ;
#9441 = LINE ( 'NONE', #21433, #903 ) ;
#9442 = EDGE_CURVE ( 'NONE', #8119, #16676, #16851, .T. ) ;
#9443 = ORIENTED_EDGE ( 'NONE', *, *, #13350, .F. ) ;
#9444 = ORIENTED_EDGE ( 'NONE', *, *, #21093, .T. ) ;
#9445 = DIRECTION ( 'NONE',  ( -6.123233995736764803E-17, 0.000000000000000000, 1.000000000000000000 ) ) ;
#9446 = DIRECTION ( 'NONE',  ( -1.000000000000000000, 0.000000000000000000, 0.000000000000000000 ) ) ;
#9447 = VERTEX_POINT ( 'NONE', #17771 ) ;
#9448 = CARTESIAN_POINT ( 'NONE',  ( -31.63662752439705272, 0.000000000000000000, 3.500000000000000000 ) ) ;
#9449 = EDGE_CURVE ( 'NONE', #3013, #19588, #10841, .T. ) ;
#9450 = VERTEX_POINT ( 'NONE', #2331 ) ;
#9451 = CARTESIAN_POINT ( 'NONE',  ( -29.69597781366221767, 56.94165929845684815, 68.75000000000000000 ) ) ;
#9452 = DIRECTION ( 'NONE',  ( 0.000000000000000000, 0.000000000000000000, 1.000000000000000000 ) ) ;
#9453 = CARTESIAN_POINT ( 'NONE',  ( -31.26086011588027347, 83.95073979834609190, 68.25000000000000000 ) ) ;
#9454 = CARTESIAN_POINT ( 'NONE',  ( -26.37540678000427619, 10.94079601157914539, 42.50000000000000000 ) ) ;
#9455 = CARTESIAN_POINT ( 'NONE',  ( 14.71174975910708049, 52.11873716947361856, 109.6002446535588319 ) ) ;
#9456 = ORIENTED_EDGE ( 'NONE', *, *, #17977, .T. ) ;
#9457 = CARTESIAN_POINT ( 'NONE',  ( -21.67365502786443088, 45.72430987248279166, 13.50000000000000000 ) ) ;
#9458 = CARTESIAN_POINT ( 'NONE',  ( 15.95292532278785913, -50.11873716947361856, 68.50000000000000000 ) ) ;
#9459 = FACE_OUTER_BOUND ( 'NONE', #10934, .T. ) ;
#9460 = FACE_OUTER_BOUND ( 'NONE', #21192, .T. ) ;
#9461 = VERTEX_POINT ( 'NONE', #3694 ) ;
#9462 = CIRCLE ( 'NONE', #174, 0.2499999999999977796 ) ;
#9463 = AXIS2_PLACEMENT_3D ( 'NONE', #16921, #21872, #1587 ) ;
#9464 = CARTESIAN_POINT ( 'NONE',  ( -14.96174975910705207, -51.86873716947361856, 68.00000000000000000 ) ) ;
#9465 = ORIENTED_EDGE ( 'NONE', *, *, #2295, .T. ) ;
#9466 = CARTESIAN_POINT ( 'NONE',  ( -15.95292532278785913, -51.61873716947361856, 14.00000000000000000 ) ) ;
#9467 = DIRECTION ( 'NONE',  ( -0.000000000000000000, -0.000000000000000000, -1.000000000000000000 ) ) ;
#9468 = VERTEX_POINT ( 'NONE', #10517 ) ;
#9469 = ORIENTED_EDGE ( 'NONE', *, *, #7343, .T. ) ;
#9470 = DIRECTION ( 'NONE',  ( 0.000000000000000000, 0.000000000000000000, -1.000000000000000000 ) ) ;
#9471 = DIRECTION ( 'NONE',  ( 1.000000000000000000, -0.000000000000000000, -0.000000000000000000 ) ) ;
#9472 = FACE_OUTER_BOUND ( 'NONE', #4574, .T. ) ;
#9473 = ORIENTED_EDGE ( 'NONE', *, *, #13448, .T. ) ;
#9474 = EDGE_CURVE ( 'NONE', #2212, #2211, #9292, .T. ) ;
#9475 = EDGE_CURVE ( 'NONE', #12787, #9842, #9277, .T. ) ;
#9476 = ORIENTED_EDGE ( 'NONE', *, *, #19586, .F. ) ;
#9477 = CARTESIAN_POINT ( 'NONE',  ( 29.37573593128808369, 68.87573593128806237, -5.214931150217776400E-15 ) ) ;
#9478 = AXIS2_PLACEMENT_3D ( 'NONE', #21795, #6473, #5109 ) ;
#9479 = VECTOR ( 'NONE', #6714, 1000.000000000000000 ) ;
#9480 = CARTESIAN_POINT ( 'NONE',  ( 23.32398829872514057, 3.528912754968628551, 13.50000000000000000 ) ) ;
#9481 = CYLINDRICAL_SURFACE ( 'NONE', #2414, 0.5999999999999999778 ) ;
#9482 = B_SPLINE_CURVE_WITH_KNOTS ( 'NONE', 3,
 ( #19430, #15514, #1878, #3902 ),
 .UNSPECIFIED., .F., .F.,
 ( 4, 4 ),
 ( 0.005071647684206891105, 0.007900577432593609145 ),
 .UNSPECIFIED. ) ;
#9483 = CARTESIAN_POINT ( 'NONE',  ( 28.57540678000427548, 6.776800961815481195, 13.50000000000000000 ) ) ;
#9484 = DIRECTION ( 'NONE',  ( 0.000000000000000000, 0.000000000000000000, -1.000000000000000000 ) ) ;
#9485 = EDGE_CURVE ( 'NONE', #1455, #2212, #15683, .T. ) ;
#9486 = CARTESIAN_POINT ( 'NONE',  ( 29.69597781366221767, 27.99124249474150972, 68.50000000000000000 ) ) ;
#9487 = LINE ( 'NONE', #5923, #235 ) ;
#9488 = CARTESIAN_POINT ( 'NONE',  ( -9.718906393579157310, 43.51045099701597252, 68.06527860057354928 ) ) ;
#9489 = ORIENTED_EDGE ( 'NONE', *, *, #8232, .T. ) ;
#9490 = FACE_OUTER_BOUND ( 'NONE', #785, .T. ) ;
#9491 = AXIS2_PLACEMENT_3D ( 'NONE', #20604, #12080, #18807 ) ;
#9492 = ADVANCED_FACE ( 'NONE', ( #20213 ), #12117, .T. ) ;
#9493 = DIRECTION ( 'NONE',  ( 1.000000000000000000, -0.000000000000000000, -0.000000000000000000 ) ) ;
#9494 = DIRECTION ( 'NONE',  ( 0.000000000000000000, 0.000000000000000000, -1.000000000000000000 ) ) ;
#9495 = CIRCLE ( 'NONE', #17361, 0.2500000000000002220 ) ;
#9496 = AXIS2_PLACEMENT_3D ( 'NONE', #10469, #9008, #3866 ) ;
#9497 = VECTOR ( 'NONE', #12582, 1000.000000000000000 ) ;
#9498 = CARTESIAN_POINT ( 'NONE',  ( -1.824728116533986810, 43.31054587065082728, 47.70876104995654288 ) ) ;
#9499 = DIRECTION ( 'NONE',  ( 1.000000000000000000, -0.000000000000000000, -0.000000000000000000 ) ) ;
#9500 = ORIENTED_EDGE ( 'NONE', *, *, #20132, .T. ) ;
#9501 = ORIENTED_EDGE ( 'NONE', *, *, #1011, .F. ) ;
#9502 = DIRECTION ( 'NONE',  ( -0.000000000000000000, -0.000000000000000000, 1.000000000000000000 ) ) ;
#9503 = ADVANCED_FACE ( 'NONE', ( #16957 ), #1409, .T. ) ;
#9504 = EDGE_CURVE ( 'NONE', #17182, #9924, #4649, .T. ) ;
#9505 = EDGE_CURVE ( 'NONE', #5446, #8176, #11807, .T. ) ;
#9506 = ORIENTED_EDGE ( 'NONE', *, *, #10479, .F. ) ;
#9507 = AXIS2_PLACEMENT_3D ( 'NONE', #5887, #16251, #2516 ) ;
#9508 = AXIS2_PLACEMENT_3D ( 'NONE', #15227, #11763, #18182 ) ;
#9509 = LINE ( 'NONE', #9402, #21290 ) ;
#9510 = ADVANCED_FACE ( 'NONE', ( #21909 ), #2859, .T. ) ;
#9511 = CARTESIAN_POINT ( 'NONE',  ( -1.774728116533986766, 42.36054587065083155, 31.80876104995653719 ) ) ;
#9512 = ORIENTED_EDGE ( 'NONE', *, *, #7782, .T. ) ;
#9513 = CARTESIAN_POINT ( 'NONE',  ( 0.000000000000000000, -85.00000000000000000, 0.000000000000000000 ) ) ;
#9514 = CIRCLE ( 'NONE', #13433, 0.05000000000000143219 ) ;
#9515 = EDGE_LOOP ( 'NONE', ( #16574, #3546, #21446, #6610 ) ) ;
#9516 = DIRECTION ( 'NONE',  ( 0.000000000000000000, 0.000000000000000000, 1.000000000000000000 ) ) ;
#9517 = PLANE ( 'NONE',  #15946 ) ;
#9518 = CARTESIAN_POINT ( 'NONE',  ( -9.141460742840918030, -32.93424481021354921, 68.50000000000000000 ) ) ;
#9519 = CARTESIAN_POINT ( 'NONE',  ( 14.71174975910705740, 42.31054587065082728, 13.50000000000000000 ) ) ;
#9520 = EDGE_CURVE ( 'NONE', #17, #6058, #7520, .T. ) ;
#9521 = LINE ( 'NONE', #16331, #13351 ) ;
#9522 = CARTESIAN_POINT ( 'NONE',  ( 26.37540678000427619, 10.94079601157914539, 42.50000000000000000 ) ) ;
#9523 = VECTOR ( 'NONE', #15484, 1000.000000000000000 ) ;
#9524 = DIRECTION ( 'NONE',  ( -0.000000000000000000, -0.000000000000000000, -1.000000000000000000 ) ) ;
#9525 = TOROIDAL_SURFACE ( 'NONE', #18824, 0.05000000000000000278, 0.05000000000000000278 ) ;
#9526 = AXIS2_PLACEMENT_3D ( 'NONE', #18748, #21796, #16609 ) ;
#9527 = AXIS2_PLACEMENT_3D ( 'NONE', #1301, #2774, #9611 ) ;
#9528 = ORIENTED_EDGE ( 'NONE', *, *, #16182, .T. ) ;
#9529 = DIRECTION ( 'NONE',  ( -0.000000000000000000, -0.000000000000000000, -1.000000000000000000 ) ) ;
#9530 = CARTESIAN_POINT ( 'NONE',  ( -8.134906293162361024, 41.92645089659918511, 68.06527860057354928 ) ) ;
#9531 = ORIENTED_EDGE ( 'NONE', *, *, #14394, .F. ) ;
#9532 = AXIS2_PLACEMENT_3D ( 'NONE', #13112, #11209, #1032 ) ;
#9533 = ORIENTED_EDGE ( 'NONE', *, *, #20885, .T. ) ;
#9534 = FACE_OUTER_BOUND ( 'NONE', #4223, .T. ) ;
#9535 = VERTEX_POINT ( 'NONE', #75 ) ;
#9536 = EDGE_CURVE ( 'NONE', #12188, #2755, #18641, .T. ) ;
#9537 = ORIENTED_EDGE ( 'NONE', *, *, #6404, .F. ) ;
#9538 = EDGE_CURVE ( 'NONE', #6564, #11436, #6922, .T. ) ;
#9539 = AXIS2_PLACEMENT_3D ( 'NONE', #10354, #12003, #8233 ) ;
#9540 = AXIS2_PLACEMENT_3D ( 'NONE', #18672, #11733, #9960 ) ;
#9541 = AXIS2_PLACEMENT_3D ( 'NONE', #2929, #18466, #9757 ) ;
#9542 = EDGE_LOOP ( 'NONE', ( #3709, #17786, #574, #19424 ) ) ;
#9543 = CIRCLE ( 'NONE', #7055, 0.3000000000000003775 ) ;
#9544 = CARTESIAN_POINT ( 'NONE',  ( 15.21174975910705918, -52.39333383871510108, 13.50000000000000000 ) ) ;
#9545 = DIRECTION ( 'NONE',  ( -0.000000000000000000, -0.000000000000000000, -1.000000000000000000 ) ) ;
#9546 = AXIS2_PLACEMENT_3D ( 'NONE', #18638, #1751, #13808 ) ;
#9547 = ORIENTED_EDGE ( 'NONE', *, *, #17425, .F. ) ;
#9548 = DIRECTION ( 'NONE',  ( 0.000000000000000000, 0.000000000000000000, -1.000000000000000000 ) ) ;
#9549 = DIRECTION ( 'NONE',  ( -1.000000000000000000, 0.000000000000000000, 0.000000000000000000 ) ) ;
#9550 = DIRECTION ( 'NONE',  ( 0.000000000000000000, 0.000000000000000000, 1.000000000000000000 ) ) ;
#9551 = CARTESIAN_POINT ( 'NONE',  ( -1.724728116533986721, 42.31054587065082728, 51.80876104995653719 ) ) ;
#9552 = DIRECTION ( 'NONE',  ( -1.734723475976806848E-16, 0.000000000000000000, 1.000000000000000000 ) ) ;
#9553 = ADVANCED_FACE ( 'NONE', ( #3322 ), #3426, .F. ) ;
#9554 = VERTEX_POINT ( 'NONE', #21802 ) ;
#9555 = CARTESIAN_POINT ( 'NONE',  ( -28.87540678000427619, 63.74634676501045050, 13.50000000000000000 ) ) ;
#9556 = DIRECTION ( 'NONE',  ( 0.9729678061520319332, 0.2309407893632090258, -0.000000000000000000 ) ) ;
#9557 = EDGE_CURVE ( 'NONE', #225, #15133, #10261, .T. ) ;
#9558 = ORIENTED_EDGE ( 'NONE', *, *, #8072, .T. ) ;
#9559 = AXIS2_PLACEMENT_3D ( 'NONE', #7500, #2110, #7701 ) ;
#9560 = TOROIDAL_SURFACE ( 'NONE', #21004, 0.05000000000000000278, 0.05000000000000000278 ) ;
#9561 = VERTEX_POINT ( 'NONE', #8144 ) ;
#9562 = VERTEX_POINT ( 'NONE', #4780 ) ;
#9563 = DIRECTION ( 'NONE',  ( -0.000000000000000000, -0.000000000000000000, 1.000000000000000000 ) ) ;
#9564 = DIRECTION ( 'NONE',  ( 0.000000000000000000, 0.000000000000000000, -1.000000000000000000 ) ) ;
#9565 = VERTEX_POINT ( 'NONE', #13610 ) ;
#9566 = AXIS2_PLACEMENT_3D ( 'NONE', #11227, #14805, #16384 ) ;
#9567 = CARTESIAN_POINT ( 'NONE',  ( 1.824728116533979261, 43.31054587065082728, 51.70876104995653577 ) ) ;
#9568 = AXIS2_PLACEMENT_3D ( 'NONE', #20086, #12898, #2725 ) ;
#9569 = EDGE_CURVE ( 'NONE', #13326, #20437, #8934, .T. ) ;
#9570 = ORIENTED_EDGE ( 'NONE', *, *, #5963, .F. ) ;
#9571 = CARTESIAN_POINT ( 'NONE',  ( 1.824728116533979705, 43.26054587065083012, 49.66679706732590915 ) ) ;
#9572 = DIRECTION ( 'NONE',  ( 0.000000000000000000, 0.000000000000000000, 1.000000000000000000 ) ) ;
#9573 = FACE_OUTER_BOUND ( 'NONE', #10282, .T. ) ;
#9574 = CYLINDRICAL_SURFACE ( 'NONE', #10236, 1.000000000000000888 ) ;
#9575 = CIRCLE ( 'NONE', #12412, 0.04999999999999991257 ) ;
#9576 = AXIS2_PLACEMENT_3D ( 'NONE', #12579, #19318, #723 ) ;
#9577 = AXIS2_PLACEMENT_3D ( 'NONE', #10288, #4914, #1778 ) ;
#9578 = DIRECTION ( 'NONE',  ( 0.000000000000000000, 0.000000000000000000, -1.000000000000000000 ) ) ;
#9579 = DIRECTION ( 'NONE',  ( 0.000000000000000000, -0.000000000000000000, 1.000000000000000000 ) ) ;
#9580 = VERTEX_POINT ( 'NONE', #9816 ) ;
#9581 = DIRECTION ( 'NONE',  ( 0.000000000000000000, 0.000000000000000000, 1.000000000000000000 ) ) ;
#9582 = DIRECTION ( 'NONE',  ( -4.336808689941893885E-15, 0.000000000000000000, 1.000000000000000000 ) ) ;
#9583 = CARTESIAN_POINT ( 'NONE',  ( 1.724728116533979616, 43.31054587065082728, 43.70876104995653577 ) ) ;
#9584 = AXIS2_PLACEMENT_3D ( 'NONE', #10740, #17321, #648 ) ;
#9585 = CARTESIAN_POINT ( 'NONE',  ( -1.774728116533986544, 43.26054587065083012, 47.80876104995653719 ) ) ;
#9586 = CARTESIAN_POINT ( 'NONE',  ( 32.50000000000002132, -71.00000000000001421, 3.200000000000000178 ) ) ;
#9587 = ORIENTED_EDGE ( 'NONE', *, *, #16432, .T. ) ;
#9588 = CARTESIAN_POINT ( 'NONE',  ( 33.49999999999999289, 84.70000000000001705, 1.799999999999996048 ) ) ;
#9589 = AXIS2_PLACEMENT_3D ( 'NONE', #11865, #6751, #11968 ) ;
#9590 = PLANE ( 'NONE',  #13201 ) ;
#9591 = AXIS2_PLACEMENT_3D ( 'NONE', #13618, #7140, #3560 ) ;
#9592 = EDGE_CURVE ( 'NONE', #9336, #15183, #1293, .T. ) ;
#9593 = ORIENTED_EDGE ( 'NONE', *, *, #14187, .T. ) ;
#9594 = CYLINDRICAL_SURFACE ( 'NONE', #13741, 0.04999999999999991257 ) ;
#9595 = CARTESIAN_POINT ( 'NONE',  ( -23.02398829872513275, -3.262363296411949332, 13.79999999999999361 ) ) ;
#9596 = ADVANCED_FACE ( 'NONE', ( #3211 ), #15165, .T. ) ;
#9597 = ORIENTED_EDGE ( 'NONE', *, *, #9356, .F. ) ;
#9598 = ORIENTED_EDGE ( 'NONE', *, *, #16448, .F. ) ;
#9599 = FACE_OUTER_BOUND ( 'NONE', #2885, .T. ) ;
#9600 = DIRECTION ( 'NONE',  ( 0.000000000000000000, 1.000000000000000000, 0.000000000000000000 ) ) ;
#9601 = CIRCLE ( 'NONE', #14895, 0.3000000000000016542 ) ;
#9602 = AXIS2_PLACEMENT_3D ( 'NONE', #18709, #1817, #3382 ) ;
#9603 = VERTEX_POINT ( 'NONE', #11701 ) ;
#9604 = AXIS2_PLACEMENT_3D ( 'NONE', #2199, #10391, #4004 ) ;
#9605 = ORIENTED_EDGE ( 'NONE', *, *, #14065, .F. ) ;
#9606 = VECTOR ( 'NONE', #13578, 1000.000000000000000 ) ;
#9607 = CIRCLE ( 'NONE', #1360, 0.2999999999999999334 ) ;
#9608 = AXIS2_PLACEMENT_3D ( 'NONE', #7266, #12262, #2213 ) ;
#9609 = CARTESIAN_POINT ( 'NONE',  ( -15.21174975910705207, 51.86873716947361856, 68.00000000000000000 ) ) ;
#9610 = DIRECTION ( 'NONE',  ( 0.000000000000000000, -1.000000000000000000, 0.000000000000000000 ) ) ;
#9611 = DIRECTION ( 'NONE',  ( 0.000000000000000000, 0.000000000000000000, 1.000000000000000000 ) ) ;
#9612 = EDGE_CURVE ( 'NONE', #5394, #583, #18220, .T. ) ;
#9613 = DIRECTION ( 'NONE',  ( -0.000000000000000000, -0.000000000000000000, -1.000000000000000000 ) ) ;
#9614 = CARTESIAN_POINT ( 'NONE',  ( -1.724728116533986721, 43.31054587065082728, 43.70876104995653577 ) ) ;
#9615 = DIRECTION ( 'NONE',  ( -1.000000000000000000, 0.000000000000000000, 0.000000000000000000 ) ) ;
#9616 = CARTESIAN_POINT ( 'NONE',  ( -14.96174975910705207, 41.81054587065082728, 68.25000000000000000 ) ) ;
#9617 = DIRECTION ( 'NONE',  ( 0.000000000000000000, 0.000000000000000000, 1.000000000000000000 ) ) ;
#9618 = VERTEX_POINT ( 'NONE', #8909 ) ;
#9619 = CIRCLE ( 'NONE', #21061, 0.2999999999999999334 ) ;
#9620 = DIRECTION ( 'NONE',  ( 0.000000000000000000, 0.000000000000000000, 1.000000000000000000 ) ) ;
#9621 = ADVANCED_FACE ( 'NONE', ( #13927 ), #9654, .F. ) ;
#9622 = EDGE_CURVE ( 'NONE', #9132, #11560, #9295, .T. ) ;
#9623 = CARTESIAN_POINT ( 'NONE',  ( -3.627054932750481964, 32.61873716947361856, 7.321391277662001151 ) ) ;
#9624 = DIRECTION ( 'NONE',  ( 0.000000000000000000, -0.000000000000000000, -1.000000000000000000 ) ) ;
#9625 = VERTEX_POINT ( 'NONE', #1952 ) ;
#9626 = CIRCLE ( 'NONE', #21067, 5.000000000000004441 ) ;
#9627 = PLANE ( 'NONE',  #7778 ) ;
#9628 = ORIENTED_EDGE ( 'NONE', *, *, #1456, .F. ) ;
#9629 = ORIENTED_EDGE ( 'NONE', *, *, #609, .F. ) ;
#9630 = DIRECTION ( 'NONE',  ( 0.000000000000000000, 0.000000000000000000, -1.000000000000000000 ) ) ;
#9631 = ITEM_DEFINED_TRANSFORMATION ( 'NONE', 'NONE', #8730,  #17493 ) ;
#9632 = ORIENTED_EDGE ( 'NONE', *, *, #15442, .T. ) ;
#9633 = ADVANCED_FACE ( 'NONE', ( #2182 ), #15717, .T. ) ;
#9634 = DIRECTION ( 'NONE',  ( -1.000000000000000000, -0.000000000000000000, -0.000000000000000000 ) ) ;
#9635 = EDGE_LOOP ( 'NONE', ( #11738, #3162, #11599, #20572, #18982, #20876, #9426, #3445 ) ) ;
#9636 = LINE ( 'NONE', #1114, #18844 ) ;
#9637 = VECTOR ( 'NONE', #19028, 1000.000000000000000 ) ;
#9638 = ORIENTED_EDGE ( 'NONE', *, *, #2118, .F. ) ;
#9639 = CARTESIAN_POINT ( 'NONE',  ( -18.22752199202934520, -38.74634676501045760, 13.79999999999999893 ) ) ;
#9640 = CARTESIAN_POINT ( 'NONE',  ( -25.37540678000427263, -68.74634676501045760, 7.200000000000000178 ) ) ;
#9641 = DIRECTION ( 'NONE',  ( 1.000000000000000000, 0.000000000000000000, -0.000000000000000000 ) ) ;
#9642 = DIRECTION ( 'NONE',  ( 1.000000000000000000, 0.000000000000000000, 0.000000000000000000 ) ) ;
#9643 = PLANE ( 'NONE',  #17885 ) ;
#9644 = EDGE_CURVE ( 'NONE', #14279, #15161, #17146, .T. ) ;
#9645 = DIRECTION ( 'NONE',  ( 0.000000000000000000, 1.000000000000000000, 0.000000000000000000 ) ) ;
#9646 = EDGE_CURVE ( 'NONE', #15986, #10680, #5006, .T. ) ;
#9647 = DIRECTION ( 'NONE',  ( 1.000000000000000000, 0.000000000000000000, 0.000000000000000000 ) ) ;
#9648 = LINE ( 'NONE', #14772, #7321 ) ;
#9649 = CIRCLE ( 'NONE', #7866, 0.6999999999999992895 ) ;
#9650 = ORIENTED_EDGE ( 'NONE', *, *, #16045, .F. ) ;
#9651 = DIRECTION ( 'NONE',  ( 1.000000000000000000, 0.000000000000000000, 0.000000000000000000 ) ) ;
#9652 = AXIS2_PLACEMENT_3D ( 'NONE', #15641, #316, #10835 ) ;
#9653 = AXIS2_PLACEMENT_3D ( 'NONE', #3840, #17478, #11881 ) ;
#9654 = TOROIDAL_SURFACE ( 'NONE', #7870, 5.300000000000004263, 0.2999999999999999889 ) ;
#9655 = PRODUCT ( 'Light', 'Light', '', ( #4257 ) ) ;
#9656 = DIRECTION ( 'NONE',  ( 0.000000000000000000, -0.000000000000000000, -1.000000000000000000 ) ) ;
#9657 = ORIENTED_EDGE ( 'NONE', *, *, #12501, .T. ) ;
#9658 = ORIENTED_EDGE ( 'NONE', *, *, #825, .F. ) ;
#9659 = CARTESIAN_POINT ( 'NONE',  ( 1.774728116533973665, 42.31054587065082728, 8.000000000000000000 ) ) ;
#9660 = CYLINDRICAL_SURFACE ( 'NONE', #14918, 0.05000000000000143219 ) ;
#9661 = ORIENTED_EDGE ( 'NONE', *, *, #19128, .T. ) ;
#9662 = ORIENTED_EDGE ( 'NONE', *, *, #21556, .T. ) ;
#9663 = EDGE_CURVE ( 'NONE', #20330, #445, #17494, .T. ) ;
#9664 = ORIENTED_EDGE ( 'NONE', *, *, #21217, .T. ) ;
#9665 = ORIENTED_EDGE ( 'NONE', *, *, #2699, .T. ) ;
#9666 = VECTOR ( 'NONE', #21661, 1000.000000000000000 ) ;
#9667 = CIRCLE ( 'NONE', #1425, 2.000000000000000000 ) ;
#9668 = LINE ( 'NONE', #19964, #8476 ) ;
#9669 = AXIS2_PLACEMENT_3D ( 'NONE', #14242, #7551, #5769 ) ;
#9670 = CARTESIAN_POINT ( 'NONE',  ( -25.37540678000427263, 63.74634676501045050, 3.500000000000000000 ) ) ;
#9671 = EDGE_LOOP ( 'NONE', ( #11037, #1766, #19463, #2788 ) ) ;
#9672 = CARTESIAN_POINT ( 'NONE',  ( 14.96174975910705918, 50.19799549595485644, 13.05380965755522737 ) ) ;
#9673 = EDGE_CURVE ( 'NONE', #8135, #21878, #6453, .T. ) ;
#9674 = DIRECTION ( 'NONE',  ( 3.052134192567367925E-16, -1.000000000000000000, 0.000000000000000000 ) ) ;
#9675 = EDGE_CURVE ( 'NONE', #17208, #15395, #17395, .T. ) ;
#9676 = DIRECTION ( 'NONE',  ( 0.000000000000000000, 0.000000000000000000, 1.000000000000000000 ) ) ;
#9677 = DIRECTION ( 'NONE',  ( -1.000000000000000000, 0.000000000000000000, 0.000000000000000000 ) ) ;
#9678 = EDGE_CURVE ( 'NONE', #2728, #3697, #10379, .T. ) ;
#9679 = ORIENTED_EDGE ( 'NONE', *, *, #9305, .T. ) ;
#9680 = DIRECTION ( 'NONE',  ( 1.000000000000000000, -0.000000000000000000, -0.000000000000000000 ) ) ;
#9681 = ORIENTED_EDGE ( 'NONE', *, *, #14104, .T. ) ;
#9682 = EDGE_LOOP ( 'NONE', ( #10450, #17835, #11306, #1565 ) ) ;
#9683 = ORIENTED_EDGE ( 'NONE', *, *, #21370, .T. ) ;
#9684 = CYLINDRICAL_SURFACE ( 'NONE', #14921, 0.5000000000000004441 ) ;
#9685 = AXIS2_PLACEMENT_3D ( 'NONE', #17671, #5847, #12115 ) ;
#9686 = LINE ( 'NONE', #17719, #2402 ) ;
#9687 = VERTEX_POINT ( 'NONE', #13811 ) ;
#9688 = AXIS2_PLACEMENT_3D ( 'NONE', #789, #7634, #11084 ) ;
#9689 = LINE ( 'NONE', #21557, #2775 ) ;
#9690 = ORIENTED_EDGE ( 'NONE', *, *, #20167, .F. ) ;
#9691 = DIRECTION ( 'NONE',  ( 0.000000000000000000, 0.000000000000000000, -1.000000000000000000 ) ) ;
#9692 = DIRECTION ( 'NONE',  ( -2.107255972849994642E-16, 0.000000000000000000, -1.000000000000000000 ) ) ;
#9693 = ADVANCED_FACE ( 'NONE', ( #3757 ), #7238, .F. ) ;
#9694 = CARTESIAN_POINT ( 'NONE',  ( 23.02398829872513986, -3.528912754968634768, 13.79999999999999893 ) ) ;
#9695 = DIRECTION ( 'NONE',  ( 0.000000000000000000, -0.000000000000000000, -1.000000000000000000 ) ) ;
#9696 = EDGE_LOOP ( 'NONE', ( #14415, #3937, #7954, #18380 ) ) ;
#9697 = DIRECTION ( 'NONE',  ( -1.000000000000000000, -0.000000000000000000, -0.000000000000000000 ) ) ;
#9698 = DIRECTION ( 'NONE',  ( 0.000000000000000000, 0.000000000000000000, 1.000000000000000000 ) ) ;
#9699 = AXIS2_PLACEMENT_3D ( 'NONE', #6148, #11155, #17979 ) ;
#9700 = DIRECTION ( 'NONE',  ( 0.000000000000000000, 0.000000000000000000, 1.000000000000000000 ) ) ;
#9701 = CARTESIAN_POINT ( 'NONE',  ( 0.000000000000000000, 71.70000000000001705, 1.800000000000000044 ) ) ;
#9702 = ORIENTED_EDGE ( 'NONE', *, *, #6225, .T. ) ;
#9703 = CARTESIAN_POINT ( 'NONE',  ( 1.824728116533979261, 42.36054587065083155, 43.70876104995653577 ) ) ;
#9704 = FACE_OUTER_BOUND ( 'NONE', #12147, .T. ) ;
#9705 = ADVANCED_FACE ( 'NONE', ( #3549 ), #3586, .F. ) ;
#9706 = VERTEX_POINT ( 'NONE', #14135 ) ;
#9707 = CARTESIAN_POINT ( 'NONE',  ( 26.61833302554978786, 9.663695060508649348, 13.50000000000000000 ) ) ;
#9708 = CARTESIAN_POINT ( 'NONE',  ( -23.02398829872514696, -2.191346223869593768, 13.32987162994455232 ) ) ;
#9709 = ORIENTED_EDGE ( 'NONE', *, *, #307, .F. ) ;
#9710 = ORIENTED_EDGE ( 'NONE', *, *, #15865, .T. ) ;
#9711 = ORIENTED_EDGE ( 'NONE', *, *, #5367, .F. ) ;
#9712 = CARTESIAN_POINT ( 'NONE',  ( -1.774728116533986544, 43.31054587065082728, 35.80876104995653009 ) ) ;
#9713 = CARTESIAN_POINT ( 'NONE',  ( 9.141460742840918030, 32.61873716947361856, 7.321391277662001151 ) ) ;
#9714 = AXIS2_PLACEMENT_3D ( 'NONE', #20975, #15809, #14122 ) ;
#9715 = CYLINDRICAL_SURFACE ( 'NONE', #2452, 1.000000000000000888 ) ;
#9716 = AXIS2_PLACEMENT_3D ( 'NONE', #6441, #8220, #8106 ) ;
#9717 = EDGE_LOOP ( 'NONE', ( #7497, #8401, #17721, #19948 ) ) ;
#9718 = ORIENTED_EDGE ( 'NONE', *, *, #21673, .F. ) ;
#9719 = CARTESIAN_POINT ( 'NONE',  ( 27.67540678000426269, 36.74634676501047181, 13.79999999999999893 ) ) ;
#9720 = EDGE_CURVE ( 'NONE', #18664, #9049, #18948, .T. ) ;
#9721 = LINE ( 'NONE', #21809, #10987 ) ;
#9722 = CARTESIAN_POINT ( 'NONE',  ( -23.02398829872513986, -2.279872152331584356, 13.43073953831958889 ) ) ;
#9723 = CARTESIAN_POINT ( 'NONE',  ( -9.178906393579158163, 42.46645089659918426, 68.06527860057354928 ) ) ;
#9724 = EDGE_CURVE ( 'NONE', #2805, #9117, #11772, .T. ) ;
#9725 = CARTESIAN_POINT ( 'NONE',  ( 1.724728116533979616, 43.31054587065082728, 37.76679706732590347 ) ) ;
#9726 = FACE_OUTER_BOUND ( 'NONE', #7799, .T. ) ;
#9727 = CARTESIAN_POINT ( 'NONE',  ( 34.69999999999999574, 85.00000000000000000, 3.009745230819759520E-15 ) ) ;
#9728 = VECTOR ( 'NONE', #9777, 1000.000000000000000 ) ;
#9729 = AXIS2_PLACEMENT_3D ( 'NONE', #10004, #18834, #3510 ) ;
#9730 = DIRECTION ( 'NONE',  ( -0.000000000000000000, 1.000000000000000000, 0.000000000000000000 ) ) ;
#9731 = DIRECTION ( 'NONE',  ( 1.000000000000000000, 0.000000000000000000, 0.000000000000000000 ) ) ;
#9732 = ORIENTED_EDGE ( 'NONE', *, *, #10048, .F. ) ;
#9733 = CARTESIAN_POINT ( 'NONE',  ( 1.774728116533973665, 43.26054587065083012, 8.000000000000000000 ) ) ;
#9734 = CARTESIAN_POINT ( 'NONE',  ( 29.50000000000002132, 0.000000000000000000, -150.0833101980363722 ) ) ;
#9735 = VERTEX_POINT ( 'NONE', #7459 ) ;
#9736 = CARTESIAN_POINT ( 'NONE',  ( -17.45292532278785913, 34.11873716947361856, 68.50000000000000000 ) ) ;
#9737 = DIRECTION ( 'NONE',  ( 0.000000000000000000, 0.000000000000000000, -1.000000000000000000 ) ) ;
#9738 = ORIENTED_EDGE ( 'NONE', *, *, #520, .F. ) ;
#9739 = EDGE_CURVE ( 'NONE', #20557, #3842, #10376, .T. ) ;
#9740 = ORIENTED_EDGE ( 'NONE', *, *, #5153, .F. ) ;
#9741 = CARTESIAN_POINT ( 'NONE',  ( 0.000000000000000000, 52.10286008774954780, 13.87500000000000000 ) ) ;
#9742 = CIRCLE ( 'NONE', #4022, 0.2999999999999999334 ) ;
#9743 = AXIS2_PLACEMENT_3D ( 'NONE', #20349, #10055, #85 ) ;
#9744 = ORIENTED_EDGE ( 'NONE', *, *, #1136, .T. ) ;
#9745 = CARTESIAN_POINT ( 'NONE',  ( 3.985331397971318079, 42.46645089659917716, 69.50000000000000000 ) ) ;
#9746 = AXIS2_PLACEMENT_3D ( 'NONE', #15783, #10768, #20844 ) ;
#9747 = CARTESIAN_POINT ( 'NONE',  ( -1.724728116533986721, 42.31054587065082728, 49.66679706732590915 ) ) ;
#9748 = DIRECTION ( 'NONE',  ( 0.9729678061520478094, 0.2309407893631419961, 0.000000000000000000 ) ) ;
#9749 = CARTESIAN_POINT ( 'NONE',  ( -1.724728116533986721, 43.26054587065083012, 53.66679706732590915 ) ) ;
#9750 = DIRECTION ( 'NONE',  ( -0.000000000000000000, -1.000000000000000000, -0.000000000000000000 ) ) ;
#9751 = DIRECTION ( 'NONE',  ( 0.000000000000000000, 0.000000000000000000, 1.000000000000000000 ) ) ;
#9752 = LINE ( 'NONE', #9307, #15455 ) ;
#9753 = DIRECTION ( 'NONE',  ( 1.000000000000000000, 0.000000000000000000, 0.000000000000000000 ) ) ;
#9754 = CARTESIAN_POINT ( 'NONE',  ( 29.01849620351543280, -6.499161877189502334, 7.532606289305298297 ) ) ;
#9755 = EDGE_CURVE ( 'NONE', #1923, #8135, #10577, .T. ) ;
#9756 = ORIENTED_EDGE ( 'NONE', *, *, #9234, .T. ) ;
#9757 = DIRECTION ( 'NONE',  ( 0.000000000000000000, 0.000000000000000000, -1.000000000000000000 ) ) ;
#9758 = EDGE_LOOP ( 'NONE', ( #18360, #20796, #7106, #10265 ) ) ;
#9759 = CARTESIAN_POINT ( 'NONE',  ( -26.37540678000427619, 10.94079601157914539, 13.50000000000000000 ) ) ;
#9760 = DIRECTION ( 'NONE',  ( 0.000000000000000000, 0.000000000000000000, -1.000000000000000000 ) ) ;
#9761 = ORIENTED_EDGE ( 'NONE', *, *, #10627, .F. ) ;
#9762 = ORIENTED_EDGE ( 'NONE', *, *, #21477, .T. ) ;
#9763 = PLANE ( 'NONE',  #274 ) ;
#9764 = SURFACE_SIDE_STYLE ('',( #2937 ) ) ;
#9765 = UNCERTAINTY_MEASURE_WITH_UNIT (LENGTH_MEASURE( 1.000000000000000082E-05 ), #9986, 'distance_accuracy_value', 'NONE');
#9766 = ORIENTED_EDGE ( 'NONE', *, *, #6209, .F. ) ;
#9767 = CARTESIAN_POINT ( 'NONE',  ( 0.000000000000000000, 0.000000000000000000, 0.000000000000000000 ) ) ;
#9768 = EDGE_CURVE ( 'NONE', #9360, #8651, #6083, .T. ) ;
#9769 = VERTEX_POINT ( 'NONE', #21552 ) ;
#9770 = EDGE_CURVE ( 'NONE', #11756, #3327, #6883, .T. ) ;
#9771 = VERTEX_POINT ( 'NONE', #6111 ) ;
#9772 = CARTESIAN_POINT ( 'NONE',  ( -15.05469906388002777, -52.39333383871510108, 13.49999999999999822 ) ) ;
#9773 = FACE_OUTER_BOUND ( 'NONE', #21436, .T. ) ;
#9774 = ORIENTED_EDGE ( 'NONE', *, *, #4070, .T. ) ;
#9775 =( NAMED_UNIT ( * ) SI_UNIT ( $, .STERADIAN. ) SOLID_ANGLE_UNIT ( ) );
#9776 = DIRECTION ( 'NONE',  ( 0.000000000000000000, -1.000000000000000000, 0.000000000000000000 ) ) ;
#9777 = DIRECTION ( 'NONE',  ( 0.000000000000000000, -0.000000000000000000, -1.000000000000000000 ) ) ;
#9778 = STYLED_ITEM ( 'NONE', ( #16564 ), #20354 ) ;
#9779 = CARTESIAN_POINT ( 'NONE',  ( -23.05541308335691042, 2.330322924046646538, 13.28711303755810214 ) ) ;
#9780 = EDGE_CURVE ( 'NONE', #1350, #20894, #7665, .T. ) ;
#9781 = CARTESIAN_POINT ( 'NONE',  ( -1.724728116533986721, 42.36054587065083155, 41.66679706732590915 ) ) ;
#9782 = ORIENTED_EDGE ( 'NONE', *, *, #5787, .T. ) ;
#9783 = ORIENTED_EDGE ( 'NONE', *, *, #3962, .T. ) ;
#9784 = ORIENTED_EDGE ( 'NONE', *, *, #15854, .F. ) ;
#9785 = FACE_OUTER_BOUND ( 'NONE', #18379, .T. ) ;
#9786 = CARTESIAN_POINT ( 'NONE',  ( 33.19999999999999574, 85.00000000000000000, 1.799999999999996048 ) ) ;
#9787 = ORIENTED_EDGE ( 'NONE', *, *, #20246, .F. ) ;
#9788 = DIRECTION ( 'NONE',  ( 0.000000000000000000, 0.000000000000000000, 1.000000000000000000 ) ) ;
#9789 = EDGE_CURVE ( 'NONE', #20854, #17559, #12668, .T. ) ;
#9790 = ADVANCED_FACE ( 'NONE', ( #11340 ), #4084, .T. ) ;
#9791 = VERTEX_POINT ( 'NONE', #930 ) ;
#9792 = CARTESIAN_POINT ( 'NONE',  ( -19.16037735075775217, 42.46645089659918426, 68.50000000000000000 ) ) ;
#9793 = CARTESIAN_POINT ( 'NONE',  ( -30.37540678000427619, 6.000000000000000000, 7.200000000000000178 ) ) ;
#9794 = ADVANCED_FACE ( 'NONE', ( #4307 ), #1051, .T. ) ;
#9795 = FACE_OUTER_BOUND ( 'NONE', #18930, .T. ) ;
#9796 = CARTESIAN_POINT ( 'NONE',  ( -34.70000000000000284, -85.00000000000000000, 0.6000000000000033085 ) ) ;
#9797 = ORIENTED_EDGE ( 'NONE', *, *, #13247, .T. ) ;
#9798 = DIRECTION ( 'NONE',  ( 0.000000000000000000, 0.000000000000000000, 1.000000000000000000 ) ) ;
#9799 = DIRECTION ( 'NONE',  ( -0.000000000000000000, 1.000000000000000000, -0.000000000000000000 ) ) ;
#9800 = AXIS2_PLACEMENT_3D ( 'NONE', #2872, #21674, #11239 ) ;
#9801 = CARTESIAN_POINT ( 'NONE',  ( -1.824728116533986810, 42.36054587065083155, 43.75876104995654003 ) ) ;
#9802 = DIRECTION ( 'NONE',  ( -0.000000000000000000, -0.000000000000000000, -1.000000000000000000 ) ) ;
#9803 = VERTEX_POINT ( 'NONE', #14697 ) ;
#9804 = CARTESIAN_POINT ( 'NONE',  ( -25.37540678000427263, -67.54634676501045476, 7.799999999999999822 ) ) ;
#9805 = CARTESIAN_POINT ( 'NONE',  ( 15.95292532278785913, -51.61873716947361856, 68.50000000000000000 ) ) ;
#9806 = EDGE_CURVE ( 'NONE', #3240, #5908, #20644, .T. ) ;
#9807 = ORIENTED_EDGE ( 'NONE', *, *, #4639, .F. ) ;
#9808 = CARTESIAN_POINT ( 'NONE',  ( 1.724728116533979616, 42.36054587065083155, 31.75876104995653648 ) ) ;
#9809 = CARTESIAN_POINT ( 'NONE',  ( -33.20000000000000284, -84.70000000000001705, 1.800000000000000266 ) ) ;
#9810 = VERTEX_POINT ( 'NONE', #2726 ) ;
#9811 = CIRCLE ( 'NONE', #6079, 0.05000000000000143219 ) ;
#9812 = ORIENTED_EDGE ( 'NONE', *, *, #9236, .T. ) ;
#9813 = EDGE_LOOP ( 'NONE', ( #6860, #13066, #6776, #7077 ) ) ;
#9814 = CARTESIAN_POINT ( 'NONE',  ( -9.641460742840918030, 32.93424481021354921, 68.00000000000000000 ) ) ;
#9815 = EDGE_CURVE ( 'NONE', #22135, #13238, #9686, .T. ) ;
#9816 = CARTESIAN_POINT ( 'NONE',  ( -29.69597781366221412, 25.99124249474150972, 68.75000000000000000 ) ) ;
#9817 = ORIENTED_EDGE ( 'NONE', *, *, #17467, .T. ) ;
#9818 = EDGE_CURVE ( 'NONE', #18311, #14054, #16375, .T. ) ;
#9819 = ORIENTED_EDGE ( 'NONE', *, *, #8311, .T. ) ;
#9820 = FACE_OUTER_BOUND ( 'NONE', #8275, .T. ) ;
#9821 = EDGE_CURVE ( 'NONE', #4856, #12853, #4550, .T. ) ;
#9822 = CARTESIAN_POINT ( 'NONE',  ( 0.000000000000000000, -32.11873716947361856, 42.50000000000000711 ) ) ;
#9823 = LINE ( 'NONE', #3102, #15973 ) ;
#9824 = DIRECTION ( 'NONE',  ( -2.388292521039847891E-16, 0.000000000000000000, -1.000000000000000000 ) ) ;
#9825 = DIRECTION ( 'NONE',  ( 0.000000000000000000, 0.000000000000000000, 1.000000000000000000 ) ) ;
#9826 = AXIS2_PLACEMENT_3D ( 'NONE', #16334, #17682, #5959 ) ;
#9827 = CARTESIAN_POINT ( 'NONE',  ( 1.724728116533979616, 43.31054587065082728, 43.80876104995653719 ) ) ;
#9828 = DIRECTION ( 'NONE',  ( 0.000000000000000000, 0.000000000000000000, 1.000000000000000000 ) ) ;
#9829 = CARTESIAN_POINT ( 'NONE',  ( 1.724728116533979616, 43.31054587065082728, 27.70876104995653577 ) ) ;
#9830 = PRODUCT_DEFINITION_SHAPE ( 'NONE', 'NONE',  #15053 ) ;
#9831 = DIRECTION ( 'NONE',  ( 1.000000000000000000, -0.000000000000000000, 6.123233995736764803E-17 ) ) ;
#9832 = ORIENTED_EDGE ( 'NONE', *, *, #12607, .F. ) ;
#9833 = CYLINDRICAL_SURFACE ( 'NONE', #4127, 0.5000000000000004441 ) ;
#9834 = CARTESIAN_POINT ( 'NONE',  ( -27.37540678000427619, 10.94079601157914539, 42.50000000000000000 ) ) ;
#9835 = LINE ( 'NONE', #16638, #4863 ) ;
#9836 = ORIENTED_EDGE ( 'NONE', *, *, #4148, .F. ) ;
#9837 = DIRECTION ( 'NONE',  ( 0.000000000000000000, 1.000000000000000000, 0.000000000000000000 ) ) ;
#9838 = EDGE_CURVE ( 'NONE', #2941, #13360, #20323, .T. ) ;
#9839 = DIRECTION ( 'NONE',  ( -1.000000000000000000, 0.000000000000000000, 0.000000000000000000 ) ) ;
#9840 = ADVANCED_FACE ( 'NONE', ( #19854 ), #16037, .T. ) ;
#9841 = AXIS2_PLACEMENT_3D ( 'NONE', #21625, #16665, #20261 ) ;
#9842 = VERTEX_POINT ( 'NONE', #1154 ) ;
#9843 = MECHANICAL_DESIGN_GEOMETRIC_PRESENTATION_REPRESENTATION (  '', ( #8411 ), #19473 ) ;
#9844 = CARTESIAN_POINT ( 'NONE',  ( 29.26816121220499411, -2.729530118891906110, -6.211574946531427711E-18 ) ) ;
#9845 = ORIENTED_EDGE ( 'NONE', *, *, #3244, .T. ) ;
#9846 = DIRECTION ( 'NONE',  ( 1.000000000000000000, 0.000000000000000000, 0.000000000000000000 ) ) ;
#9847 = CARTESIAN_POINT ( 'NONE',  ( -9.141460742840918030, -32.61873716947361856, 42.50000000000000000 ) ) ;
#9848 = AXIS2_PLACEMENT_3D ( 'NONE', #4458, #21257, #14848 ) ;
#9849 = CARTESIAN_POINT ( 'NONE',  ( 1.724728116533979838, 43.26054587065083012, 41.66679706732590915 ) ) ;
#9850 = CARTESIAN_POINT ( 'NONE',  ( -31.50000000000002132, -71.00000000000001421, 3.200000000000000178 ) ) ;
#9851 = EDGE_CURVE ( 'NONE', #12877, #4893, #7472, .T. ) ;
#9852 = DIRECTION ( 'NONE',  ( -0.000000000000000000, -0.000000000000000000, 1.000000000000000000 ) ) ;
#9853 = VECTOR ( 'NONE', #7558, 1000.000000000000000 ) ;
#9854 = CIRCLE ( 'NONE', #9149, 2.800000000000003819 ) ;
#9855 = TOROIDAL_SURFACE ( 'NONE', #14837, 6.800000000000001599, 0.2999999999999999889 ) ;
#9856 = CARTESIAN_POINT ( 'NONE',  ( -23.37634868863050031, 45.32016349109721176, 68.25000000000000000 ) ) ;
#9857 = PLANE ( 'NONE',  #3719 ) ;
#9858 = CARTESIAN_POINT ( 'NONE',  ( 9.641460742840918030, -32.61873716947361856, 42.50000000000000711 ) ) ;
#9859 = DIRECTION ( 'NONE',  ( 1.000000000000000000, 0.000000000000000000, 0.000000000000000000 ) ) ;
#9860 = DIRECTION ( 'NONE',  ( 0.000000000000000000, 0.000000000000000000, -1.000000000000000000 ) ) ;
#9861 = ORIENTED_EDGE ( 'NONE', *, *, #198, .F. ) ;
#9862 = CARTESIAN_POINT ( 'NONE',  ( -1.724728116533986721, 43.26054587065083012, 47.75876104995653293 ) ) ;
#9863 = EDGE_CURVE ( 'NONE', #17549, #4042, #21656, .T. ) ;
#9865 = FACE_OUTER_BOUND ( 'NONE', #20549, .T. ) ;
#9864 = CIRCLE ( 'NONE', #8442, 2.000000000000000000 ) ;
#9866 = ORIENTED_EDGE ( 'NONE', *, *, #12702, .T. ) ;
#9867 = ORIENTED_EDGE ( 'NONE', *, *, #20739, .F. ) ;
#9868 = CARTESIAN_POINT ( 'NONE',  ( 1.724728116533979616, 43.26054587065083012, 39.70876104995653577 ) ) ;
#9869 = CARTESIAN_POINT ( 'NONE',  ( 0.000000000000000000, 0.000000000000000000, 0.000000000000000000 ) ) ;
#9870 = VERTEX_POINT ( 'NONE', #21322 ) ;
#9871 = LINE ( 'NONE', #16680, #16427 ) ;
#9872 = VECTOR ( 'NONE', #2919, 1000.000000000000000 ) ;
#9873 = VECTOR ( 'NONE', #6902, 1000.000000000000000 ) ;
#9874 = ORIENTED_EDGE ( 'NONE', *, *, #7908, .F. ) ;
#9875 = ORIENTED_EDGE ( 'NONE', *, *, #15109, .F. ) ;
#9876 = ORIENTED_EDGE ( 'NONE', *, *, #8209, .T. ) ;
#9877 = FACE_OUTER_BOUND ( 'NONE', #4486, .T. ) ;
#9878 = EDGE_CURVE ( 'NONE', #488, #19849, #5999, .T. ) ;
#9879 = VECTOR ( 'NONE', #7087, 1000.000000000000000 ) ;
#9880 = VECTOR ( 'NONE', #7816, 1000.000000000000000 ) ;
#9881 = FACE_OUTER_BOUND ( 'NONE', #7114, .T. ) ;
#9882 = AXIS2_PLACEMENT_3D ( 'NONE', #6153, #20125, #8154 ) ;
#9883 = VERTEX_POINT ( 'NONE', #19635 ) ;
#9884 = CARTESIAN_POINT ( 'NONE',  ( -17.95292532278785913, -34.11873716947361856, 109.6002446535588319 ) ) ;
#9885 = CARTESIAN_POINT ( 'NONE',  ( 25.37540678000427263, -68.44634676501046044, 7.200000000000000178 ) ) ;
#9886 = DIRECTION ( 'NONE',  ( 1.000000000000000000, 0.000000000000000000, 0.000000000000000000 ) ) ;
#9887 = CARTESIAN_POINT ( 'NONE',  ( 0.000000000000000000, 4.700000000000000178, 3.799999999999999822 ) ) ;
#9888 = VECTOR ( 'NONE', #6082, 1000.000000000000000 ) ;
#9889 = ADVANCED_FACE ( 'NONE', ( #715 ), #7563, .T. ) ;
#9890 = CARTESIAN_POINT ( 'NONE',  ( -9.641460742840918030, 33.43424481021354921, 68.00000000000000000 ) ) ;
#9891 = VERTEX_POINT ( 'NONE', #10009 ) ;
#9892 = EDGE_LOOP ( 'NONE', ( #19138, #9113, #13695, #20128 ) ) ;
#9893 = ORIENTED_EDGE ( 'NONE', *, *, #21936, .T. ) ;
#9894 = LINE ( 'NONE', #4754, #2426 ) ;
#9895 = CARTESIAN_POINT ( 'NONE',  ( 1.824728116533979261, 43.31054587065082728, 51.80876104995653719 ) ) ;
#9896 = ORIENTED_EDGE ( 'NONE', *, *, #21899, .F. ) ;
#9897 = AXIS2_PLACEMENT_3D ( 'NONE', #13250, #4865, #18390 ) ;
#9898 = CARTESIAN_POINT ( 'NONE',  ( -1.774728116533986766, 42.36054587065083155, 31.70876104995653932 ) ) ;
#9899 = CIRCLE ( 'NONE', #4547, 0.2500000000000011657 ) ;
#9900 = ORIENTED_EDGE ( 'NONE', *, *, #14292, .F. ) ;
#9901 = FACE_OUTER_BOUND ( 'NONE', #14666, .T. ) ;
#9902 = AXIS2_PLACEMENT_3D ( 'NONE', #11698, #10575, #600 ) ;
#9903 = CARTESIAN_POINT ( 'NONE',  ( -17.45292532278785913, -50.11873716947361856, 68.50000000000000000 ) ) ;
#9904 = EDGE_CURVE ( 'NONE', #18749, #11811, #13525, .T. ) ;
#9905 = CARTESIAN_POINT ( 'NONE',  ( -1.724728116533986721, 43.26054587065083012, 43.80876104995653719 ) ) ;
#9906 = CARTESIAN_POINT ( 'NONE',  ( -15.95292532278785913, 34.11873716947361856, 68.00000000000000000 ) ) ;
#9907 = ORIENTED_EDGE ( 'NONE', *, *, #19646, .T. ) ;
#9908 = DIRECTION ( 'NONE',  ( -1.000000000000000000, 0.000000000000000000, 0.000000000000000000 ) ) ;
#9909 = DIRECTION ( 'NONE',  ( 0.000000000000000000, 0.000000000000000000, -1.000000000000000000 ) ) ;
#9910 = CARTESIAN_POINT ( 'NONE',  ( 29.69597781366221767, 58.94165929845684104, 70.50000000000000000 ) ) ;
#9911 = EDGE_LOOP ( 'NONE', ( #11836, #21876, #7852, #4407 ) ) ;
#9912 = AXIS2_PLACEMENT_3D ( 'NONE', #20704, #20590, #1664 ) ;
#9913 = AXIS2_PLACEMENT_3D ( 'NONE', #17331, #9170, #14195 ) ;
#9914 = CARTESIAN_POINT ( 'NONE',  ( -34.39999999999999858, 85.00000000000000000, 3.673940397442079220E-17 ) ) ;
#9915 = ADVANCED_FACE ( 'NONE', ( #1490 ), #4855, .F. ) ;
#9916 = ORIENTED_EDGE ( 'NONE', *, *, #15757, .F. ) ;
#9917 = CARTESIAN_POINT ( 'NONE',  ( 9.141460742840918030, 33.93424481021354921, 68.00000000000000000 ) ) ;
#9918 = EDGE_CURVE ( 'NONE', #1621, #15404, #12751, .T. ) ;
#9919 = AXIS2_PLACEMENT_3D ( 'NONE', #10263, #6588, #17081 ) ;
#9920 = LINE ( 'NONE', #3206, #10957 ) ;
#9921 = ORIENTED_EDGE ( 'NONE', *, *, #20368, .F. ) ;
#9922 = ORIENTED_EDGE ( 'NONE', *, *, #17016, .F. ) ;
#9923 = CIRCLE ( 'NONE', #1701, 0.2999999999999999334 ) ;
#9924 = VERTEX_POINT ( 'NONE', #11780 ) ;
#9925 = CARTESIAN_POINT ( 'NONE',  ( -1.824728116533986810, 43.26054587065083012, 43.80876104995653719 ) ) ;
#9926 = EDGE_CURVE ( 'NONE', #16405, #8963, #18499, .T. ) ;
#9927 = DIRECTION ( 'NONE',  ( -0.000000000000000000, -0.000000000000000000, -1.000000000000000000 ) ) ;
#9928 = VERTEX_POINT ( 'NONE', #20088 ) ;
#9929 = FACE_OUTER_BOUND ( 'NONE', #3608, .T. ) ;
#9930 = ORIENTED_EDGE ( 'NONE', *, *, #14662, .F. ) ;
#9931 = CIRCLE ( 'NONE', #14909, 0.05000000000000143219 ) ;
#9932 = DIRECTION ( 'NONE',  ( -0.000000000000000000, -0.000000000000000000, -1.000000000000000000 ) ) ;
#9933 = CIRCLE ( 'NONE', #14911, 0.2500000000000002220 ) ;
#9934 = VECTOR ( 'NONE', #18314, 1000.000000000000000 ) ;
#9935 = EDGE_CURVE ( 'NONE', #8084, #2490, #2811, .T. ) ;
#9936 = FACE_OUTER_BOUND ( 'NONE', #382, .T. ) ;
#9937 = FACE_OUTER_BOUND ( 'NONE', #16954, .T. ) ;
#9938 = DIRECTION ( 'NONE',  ( 1.000000000000000000, 0.000000000000000000, -2.388292521039847891E-16 ) ) ;
#9939 = VECTOR ( 'NONE', #17442, 1000.000000000000000 ) ;
#9940 = DIRECTION ( 'NONE',  ( 1.000000000000000000, 0.000000000000000000, 0.000000000000000000 ) ) ;
#9941 = TOROIDAL_SURFACE ( 'NONE', #20305, 0.2500000000000000000, 0.2500000000000000000 ) ;
#9942 = CYLINDRICAL_SURFACE ( 'NONE', #422, 0.2500000000000002220 ) ;
#9943 = VECTOR ( 'NONE', #11632, 1000.000000000000000 ) ;
#9944 = DIRECTION ( 'NONE',  ( -1.000000000000000000, 0.000000000000000000, -6.123233995736764803E-17 ) ) ;
#9945 = DIRECTION ( 'NONE',  ( 0.000000000000000000, -1.000000000000000000, 0.000000000000000000 ) ) ;
#9946 = DIRECTION ( 'NONE',  ( 0.000000000000000000, 0.000000000000000000, 1.000000000000000000 ) ) ;
#9947 = EDGE_LOOP ( 'NONE', ( #7037, #3817, #6783, #21527 ) ) ;
#9948 = CARTESIAN_POINT ( 'NONE',  ( 29.69597781366221767, 26.24124249474150972, 70.50000000000000000 ) ) ;
#9949 = EDGE_CURVE ( 'NONE', #18602, #17942, #6660, .T. ) ;
#9950 = CARTESIAN_POINT ( 'NONE',  ( 26.56227312273159313, 9.958410664601840878, 42.50000000000000000 ) ) ;
#9951 = AXIS2_PLACEMENT_3D ( 'NONE', #18293, #2967, #1061 ) ;
#9952 = CIRCLE ( 'NONE', #9602, 0.5000000000000004441 ) ;
#9953 = ORIENTED_EDGE ( 'NONE', *, *, #18621, .T. ) ;
#9955 = EDGE_CURVE ( 'NONE', #11408, #22089, #19252, .T. ) ;
#9954 = FACE_OUTER_BOUND ( 'NONE', #11912, .T. ) ;
#9956 = CARTESIAN_POINT ( 'NONE',  ( 14.71174975910707161, 50.19799549595485644, 68.25000000000000000 ) ) ;
#9957 = ORIENTED_EDGE ( 'NONE', *, *, #11169, .T. ) ;
#9958 = ORIENTED_EDGE ( 'NONE', *, *, #3017, .F. ) ;
#9959 = VECTOR ( 'NONE', #9502, 1000.000000000000000 ) ;
#9960 = DIRECTION ( 'NONE',  ( 0.000000000000000000, 0.000000000000000000, 1.000000000000000000 ) ) ;
#9961 = CIRCLE ( 'NONE', #2070, 2.500000000000000444 ) ;
#9962 = DIRECTION ( 'NONE',  ( 0.000000000000000000, 0.000000000000000000, 1.000000000000000000 ) ) ;
#9963 = ORIENTED_EDGE ( 'NONE', *, *, #8049, .T. ) ;
#9964 = CARTESIAN_POINT ( 'NONE',  ( -9.641460742840918030, 32.11873716947361856, 42.50000000000000711 ) ) ;
#9965 = DIRECTION ( 'NONE',  ( -0.000000000000000000, -1.000000000000000000, 0.000000000000000000 ) ) ;
#9966 = LINE ( 'NONE', #13537, #7451 ) ;
#9967 = EDGE_CURVE ( 'NONE', #8145, #9143, #659, .T. ) ;
#9968 = DIRECTION ( 'NONE',  ( 0.000000000000000000, 0.000000000000000000, -1.000000000000000000 ) ) ;
#9969 = VECTOR ( 'NONE', #11790, 1000.000000000000000 ) ;
#9970 = LINE ( 'NONE', #1793, #17136 ) ;
#9971 = DIRECTION ( 'NONE',  ( 0.000000000000000000, 0.000000000000000000, 1.000000000000000000 ) ) ;
#9972 = AXIS2_PLACEMENT_3D ( 'NONE', #21711, #9284, #7617 ) ;
#9973 = DIRECTION ( 'NONE',  ( 0.000000000000000000, 0.000000000000000000, -1.000000000000000000 ) ) ;
#9974 = CARTESIAN_POINT ( 'NONE',  ( -14.96502315657345328, -51.87273146205216534, 13.83570993898299406 ) ) ;
#9975 = CARTESIAN_POINT ( 'NONE',  ( 31.50000000000002132, 71.70000000000001705, 3.500000000000000000 ) ) ;
#9976 = ADVANCED_FACE ( 'NONE', ( #1259 ), #1683, .F. ) ;
#9977 = ORIENTED_EDGE ( 'NONE', *, *, #12935, .F. ) ;
#9978 = CARTESIAN_POINT ( 'NONE',  ( 27.67540678000428400, -10.94079601157914716, 13.79999999999999893 ) ) ;
#9979 = ORIENTED_EDGE ( 'NONE', *, *, #20001, .T. ) ;
#9980 = FACE_OUTER_BOUND ( 'NONE', #4884, .T. ) ;
#9981 = ORIENTED_EDGE ( 'NONE', *, *, #16309, .T. ) ;
#9982 = EDGE_LOOP ( 'NONE', ( #21131, #7690, #1109, #20929 ) ) ;
#9983 = CARTESIAN_POINT ( 'NONE',  ( -32.50000000000002132, 71.00000000000001421, 3.200000000000000178 ) ) ;
#9984 = ORIENTED_EDGE ( 'NONE', *, *, #18129, .T. ) ;
#9985 = CIRCLE ( 'NONE', #19266, 0.3000000000000016542 ) ;
#9986 =( LENGTH_UNIT ( ) NAMED_UNIT ( * ) SI_UNIT ( .MILLI., .METRE. ) );
#9987 = ORIENTED_EDGE ( 'NONE', *, *, #1725, .F. ) ;
#9988 = CIRCLE ( 'NONE', #3197, 0.6000000000000000888 ) ;
#9989 = ORIENTED_EDGE ( 'NONE', *, *, #5029, .T. ) ;
#9990 = ORIENTED_EDGE ( 'NONE', *, *, #7184, .T. ) ;
#9991 = EDGE_CURVE ( 'NONE', #19336, #1902, #8433, .T. ) ;
#9992 = LINE ( 'NONE', #1474, #20952 ) ;
#9993 = CARTESIAN_POINT ( 'NONE',  ( -13.75390639357915923, 42.46645089659918426, 70.38908280829822672 ) ) ;
#9994 = EDGE_CURVE ( 'NONE', #3158, #5533, #18282, .T. ) ;
#9995 = CARTESIAN_POINT ( 'NONE',  ( 24.13662752439704917, 0.000000000000000000, 3.799999999999999822 ) ) ;
#9996 = VERTEX_POINT ( 'NONE', #15035 ) ;
#9997 = CARTESIAN_POINT ( 'NONE',  ( -1.724728116533986721, 42.31054587065082728, 35.80876104995653009 ) ) ;
#9998 = AXIS2_PLACEMENT_3D ( 'NONE', #12982, #13098, #3161 ) ;
#9999 = LINE ( 'NONE', #8547, #11882 ) ;
#10000 = VECTOR ( 'NONE', #20256, 1000.000000000000000 ) ;
#10001 = DIRECTION ( 'NONE',  ( 0.000000000000000000, 0.000000000000000000, -1.000000000000000000 ) ) ;
#10002 =( BOUNDED_CURVE ( )  B_SPLINE_CURVE ( 3, ( #21568, #17738, #4423, #6232 ),
 .UNSPECIFIED., .F., .T. ) 
 B_SPLINE_CURVE_WITH_KNOTS ( ( 4, 4 ),
 ( 3.141592653589793116, 4.712388980384687009 ),
 .UNSPECIFIED. ) 
 CURVE ( )  GEOMETRIC_REPRESENTATION_ITEM ( )  RATIONAL_B_SPLINE_CURVE ( ( 1.000000000000000000, 0.8047378541243654926, 0.8047378541243654926, 1.000000000000000000 ) ) 
 REPRESENTATION_ITEM ( '' )  );
#10003 = DIRECTION ( 'NONE',  ( 0.000000000000000000, 0.000000000000000000, 1.000000000000000000 ) ) ;
#10004 = CARTESIAN_POINT ( 'NONE',  ( 0.000000000000000000, -5.000000000000000000, 7.500000000000000000 ) ) ;
#10005 = VERTEX_POINT ( 'NONE', #15248 ) ;
#10006 = ORIENTED_EDGE ( 'NONE', *, *, #1509, .F. ) ;
#10007 = EDGE_LOOP ( 'NONE', ( #10388, #13324, #13870, #10461 ) ) ;
#10008 = DIRECTION ( 'NONE',  ( -6.123233995736766036E-17, 0.000000000000000000, 1.000000000000000000 ) ) ;
#10009 = CARTESIAN_POINT ( 'NONE',  ( -35.00000000000000000, -84.70000000000001705, 0.6000000000000033085 ) ) ;
#10010 = EDGE_LOOP ( 'NONE', ( #17976, #2239, #5242, #11778 ) ) ;
#10011 = ADVANCED_FACE ( 'NONE', ( #22104 ), #6781, .F. ) ;
#10012 = LINE ( 'NONE', #10230, #199 ) ;
#10013 = APPLICATION_CONTEXT ( 'automotive_design' ) ;
#10014 = CIRCLE ( 'NONE', #1471, 2.500000000000002220 ) ;
#10015 = TOROIDAL_SURFACE ( 'NONE', #17515, 0.2999999999999999889, 0.2999999999999999889 ) ;
#10016 = VECTOR ( 'NONE', #20075, 1000.000000000000000 ) ;
#10017 = VERTEX_POINT ( 'NONE', #20182 ) ;
#10018 = DIRECTION ( 'NONE',  ( 0.000000000000000000, 0.000000000000000000, 1.000000000000000000 ) ) ;
#10019 = CARTESIAN_POINT ( 'NONE',  ( 32.50000000000002132, 71.00000000000001421, 3.200000000000000178 ) ) ;
#10020 = EDGE_CURVE ( 'NONE', #4799, #7172, #1380, .T. ) ;
#10021 = CARTESIAN_POINT ( 'NONE',  ( -30.49999999999999289, -123.9599366953518711, 9.999999999999998224 ) ) ;
#10022 = CARTESIAN_POINT ( 'NONE',  ( -28.87540678000427619, -6.494748934539263274, 13.50000000000000000 ) ) ;
#10023 = ORIENTED_EDGE ( 'NONE', *, *, #10702, .F. ) ;
#10024 = FACE_OUTER_BOUND ( 'NONE', #5373, .T. ) ;
#10025 = FACE_OUTER_BOUND ( 'NONE', #5019, .T. ) ;
#10026 = DIRECTION ( 'NONE',  ( 0.000000000000000000, 0.000000000000000000, -1.000000000000000000 ) ) ;
#10027 = CARTESIAN_POINT ( 'NONE',  ( -30.19999999999999574, 69.70000000000001705, 1.199999999999999734 ) ) ;
#10028 = DIRECTION ( 'NONE',  ( 1.000000000000000000, 0.000000000000000000, 0.000000000000000000 ) ) ;
#10029 = ORIENTED_EDGE ( 'NONE', *, *, #96, .T. ) ;
#10030 = DIRECTION ( 'NONE',  ( 0.000000000000000000, -1.000000000000000000, 0.000000000000000000 ) ) ;
#10031 = AXIS2_PLACEMENT_3D ( 'NONE', #9513, #2470, #882 ) ;
#10032 = DIRECTION ( 'NONE',  ( 0.000000000000000000, -1.000000000000000000, 0.000000000000000000 ) ) ;
#10033 = ORIENTED_EDGE ( 'NONE', *, *, #19691, .F. ) ;
#10034 = AXIS2_PLACEMENT_3D ( 'NONE', #8418, #16808, #15124 ) ;
#10035 = FACE_OUTER_BOUND ( 'NONE', #2992, .T. ) ;
#10036 = DIRECTION ( 'NONE',  ( 0.000000000000000000, 1.000000000000000000, 0.000000000000000000 ) ) ;
#10037 = VERTEX_POINT ( 'NONE', #11889 ) ;
#10038 = EDGE_LOOP ( 'NONE', ( #6060, #15866, #17872, #6088 ) ) ;
#10039 = ORIENTED_EDGE ( 'NONE', *, *, #21343, .T. ) ;
#10040 = FACE_OUTER_BOUND ( 'NONE', #15605, .T. ) ;
#10041 = EDGE_CURVE ( 'NONE', #5684, #21031, #5637, .T. ) ;
#10042 = DIRECTION ( 'NONE',  ( 1.000000000000000000, 0.000000000000000000, 0.000000000000000000 ) ) ;
#10043 = ORIENTED_EDGE ( 'NONE', *, *, #14708, .T. ) ;
#10044 = DIRECTION ( 'NONE',  ( -1.000000000000000000, 0.000000000000000000, 2.107255972849994642E-16 ) ) ;
#10045 = ORIENTED_EDGE ( 'NONE', *, *, #21285, .T. ) ;
#10046 = VERTEX_POINT ( 'NONE', #11663 ) ;
#10047 = CARTESIAN_POINT ( 'NONE',  ( -1.824728116533986810, 43.31054587065082728, 53.66679706732590915 ) ) ;
#10048 = EDGE_CURVE ( 'NONE', #13253, #6305, #18840, .T. ) ;
#10049 = EDGE_CURVE ( 'NONE', #7627, #11313, #12211, .T. ) ;
#10050 = ORIENTED_EDGE ( 'NONE', *, *, #6532, .T. ) ;
#10051 = CARTESIAN_POINT ( 'NONE',  ( -32.20000000000001705, 0.000000000000000000, 1.500000000000000000 ) ) ;
#10052 = EDGE_CURVE ( 'NONE', #833, #14107, #1741, .T. ) ;
#10053 = CARTESIAN_POINT ( 'NONE',  ( 1.774728116533979438, 42.36054587065083155, 43.70876104995653577 ) ) ;
#10054 = LINE ( 'NONE', #22027, #7164 ) ;
#10055 = DIRECTION ( 'NONE',  ( 0.000000000000000000, -0.000000000000000000, 1.000000000000000000 ) ) ;
#10056 = ORIENTED_EDGE ( 'NONE', *, *, #16883, .F. ) ;
#10057 = CARTESIAN_POINT ( 'NONE',  ( 23.32398829872514057, 7.118794219358020148E-15, 13.50000000000000000 ) ) ;
#10058 = DIRECTION ( 'NONE',  ( 0.000000000000000000, -0.000000000000000000, -1.000000000000000000 ) ) ;
#10059 = DIRECTION ( 'NONE',  ( 1.000000000000000000, 0.000000000000000000, 0.000000000000000000 ) ) ;
#10060 = ORIENTED_EDGE ( 'NONE', *, *, #7110, .F. ) ;
#10061 = CARTESIAN_POINT ( 'NONE',  ( -4.127054932750482408, -33.93424481021354921, 68.00000000000000000 ) ) ;
#10062 = CIRCLE ( 'NONE', #15752, 0.6999999999999992895 ) ;
#10063 = VECTOR ( 'NONE', #815, 1000.000000000000000 ) ;
#10064 = ORIENTED_EDGE ( 'NONE', *, *, #5728, .T. ) ;
#10065 = FACE_OUTER_BOUND ( 'NONE', #12391, .T. ) ;
#10066 = EDGE_CURVE ( 'NONE', #12623, #15917, #2036, .T. ) ;
#10067 = CARTESIAN_POINT ( 'NONE',  ( -31.44597781366221412, 27.99124249474150972, 70.50000000000000000 ) ) ;
#10068 = AXIS2_PLACEMENT_3D ( 'NONE', #611, #2293, #7136 ) ;
#10069 = EDGE_LOOP ( 'NONE', ( #10254, #17790, #3208, #9832 ) ) ;
#10070 = ORIENTED_EDGE ( 'NONE', *, *, #21277, .F. ) ;
#10071 = CARTESIAN_POINT ( 'NONE',  ( -31.50000000000002132, -71.00000000000001421, 3.500000000000000000 ) ) ;
#10072 = CIRCLE ( 'NONE', #8996, 0.2500000000000002220 ) ;
#10073 = ORIENTED_EDGE ( 'NONE', *, *, #9720, .T. ) ;
#10074 = ADVANCED_FACE ( 'NONE', ( #15894 ), #12043, .F. ) ;
#10075 = AXIS2_PLACEMENT_3D ( 'NONE', #5544, #5665, #7655 ) ;
#10076 = LINE ( 'NONE', #15094, #8860 ) ;
#10077 = CARTESIAN_POINT ( 'NONE',  ( -23.61959064016851073, 45.26242829375641463, 13.74999999999999822 ) ) ;
#10078 = CIRCLE ( 'NONE', #778, 4.999999999999997335 ) ;
#10079 = ADVANCED_FACE ( 'NONE', ( #15688 ), #20993, .T. ) ;
#10080 = FACE_OUTER_BOUND ( 'NONE', #4331, .T. ) ;
#10081 = EDGE_CURVE ( 'NONE', #8471, #13403, #361, .T. ) ;
#10082 = CARTESIAN_POINT ( 'NONE',  ( -1.824728116533986810, 43.26054587065083012, 29.66679706732590560 ) ) ;
#10083 = CARTESIAN_POINT ( 'NONE',  ( 1.724728116533979838, 42.36054587065083155, 29.71679706732590986 ) ) ;
#10084 = CARTESIAN_POINT ( 'NONE',  ( 3.127054932750481964, 32.61873716947361856, 68.00000000000000000 ) ) ;
#10085 = PLANE ( 'NONE',  #13617 ) ;
#10086 = DIRECTION ( 'NONE',  ( 0.000000000000000000, 0.000000000000000000, -1.000000000000000000 ) ) ;
#10087 = CARTESIAN_POINT ( 'NONE',  ( -32.50000000000002132, -71.00000000000001421, 1.800000000000000044 ) ) ;
#10088 = CARTESIAN_POINT ( 'NONE',  ( -10.20831163238817574, 43.00645089659918341, 70.88527860057354246 ) ) ;
#10089 = AXIS2_PLACEMENT_3D ( 'NONE', #19760, #10913, #5796 ) ;
#10090 = AXIS2_PLACEMENT_3D ( 'NONE', #14429, #19944, #16552 ) ;
#10091 = EDGE_CURVE ( 'NONE', #2915, #10170, #9091, .T. ) ;
#10092 = DIRECTION ( 'NONE',  ( 0.000000000000000000, 0.000000000000000000, 1.000000000000000000 ) ) ;
#10093 = ORIENTED_EDGE ( 'NONE', *, *, #7331, .T. ) ;
#10094 = CARTESIAN_POINT ( 'NONE',  ( 14.71174975910707161, 51.61873716947361856, 68.25000000000000000 ) ) ;
#10095 = EDGE_LOOP ( 'NONE', ( #12754, #10726, #5065, #19255 ) ) ;
#10096 = VERTEX_POINT ( 'NONE', #246 ) ;
#10097 = CYLINDRICAL_SURFACE ( 'NONE', #12422, 0.2500000000000002220 ) ;
#10098 = EDGE_CURVE ( 'NONE', #14287, #3240, #3536, .T. ) ;
#10099 = ORIENTED_EDGE ( 'NONE', *, *, #11432, .F. ) ;
#10100 = ORIENTED_EDGE ( 'NONE', *, *, #439, .T. ) ;
#10101 = ORIENTED_EDGE ( 'NONE', *, *, #13681, .F. ) ;
#10102 = ADVANCED_FACE ( 'NONE', ( #140 ), #16012, .T. ) ;
#10103 = CIRCLE ( 'NONE', #6186, 0.04999999999999991257 ) ;
#10104 = FACE_OUTER_BOUND ( 'NONE', #21296, .T. ) ;
#10105 = CARTESIAN_POINT ( 'NONE',  ( -14.96174975910705207, 51.86873716947361856, 68.00000000000000000 ) ) ;
#10106 = TOROIDAL_SURFACE ( 'NONE', #2186, 0.5000000000000000000, 0.2500000000000000000 ) ;
#10107 = DIRECTION ( 'NONE',  ( 1.000000000000000000, 0.000000000000000000, 0.000000000000000000 ) ) ;
#10108 = ORIENTED_EDGE ( 'NONE', *, *, #15287, .F. ) ;
#10109 = DIRECTION ( 'NONE',  ( 1.000000000000000000, 0.000000000000000000, 0.000000000000000000 ) ) ;
#10110 = CARTESIAN_POINT ( 'NONE',  ( -1.724728116533986721, 43.26054587065083012, 37.71679706732590631 ) ) ;
#10111 = CARTESIAN_POINT ( 'NONE',  ( -28.87540678000427619, 0.000000000000000000, 13.50000000000000000 ) ) ;
#10112 = CARTESIAN_POINT ( 'NONE',  ( 31.50000000000002132, 71.00000000000001421, 1.800000000000000044 ) ) ;
#10113 = VECTOR ( 'NONE', #19052, 1000.000000000000000 ) ;
#10114 = CARTESIAN_POINT ( 'NONE',  ( -29.13662752439705272, 0.000000000000000000, 3.500000000000000000 ) ) ;
#10115 = ORIENTED_EDGE ( 'NONE', *, *, #2372, .T. ) ;
#10116 = ORIENTED_EDGE ( 'NONE', *, *, #4233, .F. ) ;
#10117 = ORIENTED_EDGE ( 'NONE', *, *, #15622, .F. ) ;
#10118 = DIRECTION ( 'NONE',  ( 1.000000000000000000, 0.000000000000000000, 0.000000000000000000 ) ) ;
#10120 = EDGE_CURVE ( 'NONE', #675, #3754, #7105, .T. ) ;
#10119 = CARTESIAN_POINT ( 'NONE',  ( -1.724728116533986721, 43.26054587065083012, 41.71679706732590631 ) ) ;
#10121 = EDGE_CURVE ( 'NONE', #1107, #877, #1829, .T. ) ;
#10122 = EDGE_CURVE ( 'NONE', #19547, #7401, #15963, .T. ) ;
#10123 = DIRECTION ( 'NONE',  ( 0.9729678061520313781, 0.2309407893632117181, 0.000000000000000000 ) ) ;
#10124 = VERTEX_POINT ( 'NONE', #13778 ) ;
#10125 = DIRECTION ( 'NONE',  ( 0.000000000000000000, 1.000000000000000000, 0.000000000000000000 ) ) ;
#10126 = LINE ( 'NONE', #21890, #20639 ) ;
#10127 = CARTESIAN_POINT ( 'NONE',  ( 28.57540678000427548, 0.000000000000000000, 13.19999999999999929 ) ) ;
#10128 = EDGE_LOOP ( 'NONE', ( #4562, #17302, #21716, #14673 ) ) ;
#10129 = DIRECTION ( 'NONE',  ( 0.000000000000000000, -1.000000000000000000, 0.000000000000000000 ) ) ;
#10130 = CARTESIAN_POINT ( 'NONE',  ( -15.21174975910705207, -51.61873716947361856, 14.00000000000000000 ) ) ;
#10131 = CARTESIAN_POINT ( 'NONE',  ( -1.774728116533986766, 43.26054587065083012, 45.66679706732590205 ) ) ;
#10132 = SURFACE_SIDE_STYLE ('',( #8344 ) ) ;
#10133 = ORIENTED_EDGE ( 'NONE', *, *, #5717, .T. ) ;
#10134 = EDGE_CURVE ( 'NONE', #13657, #16494, #17259, .T. ) ;
#10135 = CYLINDRICAL_SURFACE ( 'NONE', #192, 0.04999999999999991257 ) ;
#10136 = ORIENTED_EDGE ( 'NONE', *, *, #3559, .F. ) ;
#10137 = CARTESIAN_POINT ( 'NONE',  ( -31.69597781366221412, 25.99124249474150972, 68.75000000000000000 ) ) ;
#10138 = DIRECTION ( 'NONE',  ( -1.000000000000000000, 0.000000000000000000, 1.442933311647907116E-16 ) ) ;
#10139 = EDGE_LOOP ( 'NONE', ( #3661, #9465, #8222, #15817 ) ) ;
#10140 = ORIENTED_EDGE ( 'NONE', *, *, #18082, .T. ) ;
#10141 = ORIENTED_EDGE ( 'NONE', *, *, #20490, .F. ) ;
#10142 = LINE ( 'NONE', #20553, #10284 ) ;
#10143 = EDGE_CURVE ( 'NONE', #13948, #12996, #15794, .T. ) ;
#10144 = DIRECTION ( 'NONE',  ( 1.000000000000000000, 0.000000000000000000, 0.000000000000000000 ) ) ;
#10145 = VERTEX_POINT ( 'NONE', #462 ) ;
#10146 = ORIENTED_EDGE ( 'NONE', *, *, #19116, .T. ) ;
#10147 = EDGE_LOOP ( 'NONE', ( #13590, #14388, #19833, #716 ) ) ;
#10148 = DIRECTION ( 'NONE',  ( -0.000000000000000000, 0.000000000000000000, 1.000000000000000000 ) ) ;
#10149 = AXIS2_PLACEMENT_3D ( 'NONE', #19327, #1968, #15616 ) ;
#10150 = ORIENTED_EDGE ( 'NONE', *, *, #12114, .F. ) ;
#10151 = CARTESIAN_POINT ( 'NONE',  ( 15.95292532278785913, 32.61873716947361856, 68.00000000000000000 ) ) ;
#10152 = LINE ( 'NONE', #1959, #2443 ) ;
#10153 = DIRECTION ( 'NONE',  ( 1.000000000000000000, 0.000000000000000000, 0.000000000000000000 ) ) ;
#10154 = CARTESIAN_POINT ( 'NONE',  ( 1.724728116533979838, 42.36054587065083155, 37.71679706732590631 ) ) ;
#10155 = ORIENTED_EDGE ( 'NONE', *, *, #10675, .T. ) ;
#10156 = DIRECTION ( 'NONE',  ( -2.832483164223434527E-16, 1.000000000000000000, 0.000000000000000000 ) ) ;
#10157 = CARTESIAN_POINT ( 'NONE',  ( -31.50000000000002132, 71.00000000000001421, 1.800000000000000044 ) ) ;
#10158 = VECTOR ( 'NONE', #14542, 1000.000000000000000 ) ;
#10159 = DIRECTION ( 'NONE',  ( 0.000000000000000000, 0.000000000000000000, 1.000000000000000000 ) ) ;
#10160 = FACE_OUTER_BOUND ( 'NONE', #9717, .T. ) ;
#10161 = LINE ( 'NONE', #6846, #7442 ) ;
#10162 = ORIENTED_EDGE ( 'NONE', *, *, #1561, .T. ) ;
#10163 = CARTESIAN_POINT ( 'NONE',  ( -14.96174975910705207, -41.81054587065082728, 13.75000000000000000 ) ) ;
#10164 = CIRCLE ( 'NONE', #14791, 2.000000000000000000 ) ;
#10165 = LINE ( 'NONE', #13399, #8797 ) ;
#10166 = ORIENTED_EDGE ( 'NONE', *, *, #20316, .T. ) ;
#10167 = PLANE ( 'NONE',  #18172 ) ;
#10168 = EDGE_CURVE ( 'NONE', #14982, #21652, #19559, .T. ) ;
#10169 = DIRECTION ( 'NONE',  ( -1.000000000000000000, 0.000000000000000000, 0.000000000000000000 ) ) ;
#10170 = VERTEX_POINT ( 'NONE', #20637 ) ;
#10171 = EDGE_CURVE ( 'NONE', #7404, #2571, #972, .T. ) ;
#10172 = ORIENTED_EDGE ( 'NONE', *, *, #15463, .T. ) ;
#10173 = CYLINDRICAL_SURFACE ( 'NONE', #14896, 1.000000000000000888 ) ;
#10174 = ORIENTED_EDGE ( 'NONE', *, *, #20848, .T. ) ;
#10175 = CIRCLE ( 'NONE', #2310, 0.09999999999999939493 ) ;
#10176 = LINE ( 'NONE', #18566, #15289 ) ;
#10177 = ORIENTED_EDGE ( 'NONE', *, *, #9251, .T. ) ;
#10178 = CARTESIAN_POINT ( 'NONE',  ( 30.49999999999999645, 69.70000000000000284, 1.753093177964017524E-15 ) ) ;
#10179 = CARTESIAN_POINT ( 'NONE',  ( -29.50000000000002132, 0.000000000000000000, 0.2999999999999947153 ) ) ;
#10180 = CARTESIAN_POINT ( 'NONE',  ( -3.627054932750481964, 32.61873716947361856, 68.00000000000000000 ) ) ;
#10181 = CARTESIAN_POINT ( 'NONE',  ( 29.13662752439705272, 0.000000000000000000, 3.799999999999999822 ) ) ;
#10182 = CARTESIAN_POINT ( 'NONE',  ( 34.99999999999999289, -84.70000000000001705, 0.6000000000000033085 ) ) ;
#10183 = EDGE_CURVE ( 'NONE', #8599, #19790, #1927, .T. ) ;
#10184 = DIRECTION ( 'NONE',  ( 1.000000000000000000, 0.000000000000000000, 0.000000000000000000 ) ) ;
#10185 = DIRECTION ( 'NONE',  ( 2.107255972849994642E-16, -0.000000000000000000, 1.000000000000000000 ) ) ;
#10186 = CARTESIAN_POINT ( 'NONE',  ( -4.127054932750482408, 33.43424481021354921, 42.50000000000000000 ) ) ;
#10187 = LINE ( 'NONE', #8194, #15078 ) ;
#10188 = CARTESIAN_POINT ( 'NONE',  ( 29.13662752439705272, -5.000000000000000000, 7.500000000000000000 ) ) ;
#10189 = AXIS2_PLACEMENT_3D ( 'NONE', #21951, #6624, #13949 ) ;
#10190 = CONICAL_SURFACE ( 'NONE', #21639, 0.9652499999999990532, 0.06981317007976590994 ) ;
#10191 = ADVANCED_FACE ( 'NONE', ( #15568 ), #802, .T. ) ;
#10192 = ORIENTED_EDGE ( 'NONE', *, *, #4398, .T. ) ;
#10193 = ADVANCED_FACE ( 'NONE', ( #7541 ), #4166, .T. ) ;
#10194 = CYLINDRICAL_SURFACE ( 'NONE', #16686, 0.2999999999999999334 ) ;
#10195 = ORIENTED_EDGE ( 'NONE', *, *, #20228, .F. ) ;
#10196 = DIRECTION ( 'NONE',  ( 0.000000000000000000, 0.000000000000000000, -1.000000000000000000 ) ) ;
#10197 = ADVANCED_FACE ( 'NONE', ( #2600 ), #9660, .T. ) ;
#10198 = DIRECTION ( 'NONE',  ( 0.000000000000000000, -0.000000000000000000, -1.000000000000000000 ) ) ;
#10199 = ORIENTED_EDGE ( 'NONE', *, *, #13644, .T. ) ;
#10200 = ORIENTED_EDGE ( 'NONE', *, *, #13630, .F. ) ;
#10201 = PLANE ( 'NONE',  #291 ) ;
#10202 = EDGE_CURVE ( 'NONE', #7888, #4947, #7755, .T. ) ;
#10203 = APPLICATION_PROTOCOL_DEFINITION ( 'draft international standard', 'automotive_design', 1998, #9155 ) ;
#10204 = ORIENTED_EDGE ( 'NONE', *, *, #2972, .T. ) ;
#10205 = PRESENTATION_STYLE_ASSIGNMENT (( #3270 ) ) ;
#10206 = VECTOR ( 'NONE', #16299, 1000.000000000000000 ) ;
#10207 = ORIENTED_EDGE ( 'NONE', *, *, #2869, .T. ) ;
#10208 = AXIS2_PLACEMENT_3D ( 'NONE', #5444, #12232, #19081 ) ;
#10209 = VERTEX_POINT ( 'NONE', #16347 ) ;
#10210 = CARTESIAN_POINT ( 'NONE',  ( 15.95292532278785913, -52.09333383871509682, 13.79999999999999893 ) ) ;
#10211 = ADVANCED_FACE ( 'NONE', ( #20338 ), #9207, .T. ) ;
#10212 = CARTESIAN_POINT ( 'NONE',  ( 15.00584427753688921, -51.86868465798484351, 13.49999999999999645 ) ) ;
#10213 = FACE_OUTER_BOUND ( 'NONE', #21668, .T. ) ;
#10214 = DIRECTION ( 'NONE',  ( 0.000000000000000000, 1.000000000000000000, 0.000000000000000000 ) ) ;
#10215 = CARTESIAN_POINT ( 'NONE',  ( 1.774728116533979883, 42.36054587065083155, 29.66679706732590560 ) ) ;
#10216 = DIRECTION ( 'NONE',  ( 0.000000000000000000, 0.000000000000000000, 1.000000000000000000 ) ) ;
#10217 = CARTESIAN_POINT ( 'NONE',  ( -9.178906393579158163, 42.46645089659918426, 68.06527860057354928 ) ) ;
#10218 = CIRCLE ( 'NONE', #14115, 0.2500000000000002220 ) ;
#10219 = DIRECTION ( 'NONE',  ( 0.000000000000000000, -0.000000000000000000, -1.000000000000000000 ) ) ;
#10220 = EDGE_CURVE ( 'NONE', #5056, #803, #253, .T. ) ;
#10221 = AXIS2_PLACEMENT_3D ( 'NONE', #5626, #20942, #21180 ) ;
#10222 = ORIENTED_EDGE ( 'NONE', *, *, #8311, .F. ) ;
#10223 = VECTOR ( 'NONE', #10030, 1000.000000000000000 ) ;
#10224 = VECTOR ( 'NONE', #7144, 1000.000000000000000 ) ;
#10225 = ORIENTED_EDGE ( 'NONE', *, *, #7618, .F. ) ;
#10226 = CARTESIAN_POINT ( 'NONE',  ( -12.06058343050541204, 42.46645089659918426, 68.75385983073485363 ) ) ;
#10227 = ADVANCED_FACE ( 'NONE', ( #13378 ), #3428, .T. ) ;
#10228 = CARTESIAN_POINT ( 'NONE',  ( 0.000000000000000000, 32.11873716947361856, 109.6002446535588319 ) ) ;
#10229 = ORIENTED_EDGE ( 'NONE', *, *, #7319, .T. ) ;
#10230 = CARTESIAN_POINT ( 'NONE',  ( 28.87540678000427619, -63.74634676501045050, 13.19999999999999929 ) ) ;
#10231 = VERTEX_POINT ( 'NONE', #6817 ) ;
#10232 = ORIENTED_EDGE ( 'NONE', *, *, #16471, .F. ) ;
#10233 = DIRECTION ( 'NONE',  ( 0.000000000000000000, 0.000000000000000000, -1.000000000000000000 ) ) ;
#10234 = CIRCLE ( 'NONE', #19158, 0.5000000000000004441 ) ;
#10235 = AXIS2_PLACEMENT_3D ( 'NONE', #1719, #1496, #18502 ) ;
#10236 = AXIS2_PLACEMENT_3D ( 'NONE', #9454, #11352, #14709 ) ;
#10237 = DIRECTION ( 'NONE',  ( 0.000000000000000000, -1.000000000000000000, 0.000000000000000000 ) ) ;
#10238 = LINE ( 'NONE', #10022, #4870 ) ;
#10239 = EDGE_LOOP ( 'NONE', ( #17968, #663, #1466, #6887 ) ) ;
#10240 = DIRECTION ( 'NONE',  ( 0.000000000000000000, 0.000000000000000000, -1.000000000000000000 ) ) ;
#10241 = FACE_OUTER_BOUND ( 'NONE', #4371, .T. ) ;
#10242 = EDGE_CURVE ( 'NONE', #4102, #20280, #20661, .T. ) ;
#10243 = DIRECTION ( 'NONE',  ( -0.000000000000000000, -1.000000000000000000, -0.000000000000000000 ) ) ;
#10244 = EDGE_CURVE ( 'NONE', #16612, #13226, #1755, .T. ) ;
#10245 = DIRECTION ( 'NONE',  ( 1.000000000000000000, 0.000000000000000000, 0.000000000000000000 ) ) ;
#10246 = DIRECTION ( 'NONE',  ( 0.000000000000000000, 1.000000000000000000, 0.000000000000000000 ) ) ;
#10247 = ORIENTED_EDGE ( 'NONE', *, *, #21088, .T. ) ;
#10248 = DIRECTION ( 'NONE',  ( -1.000000000000000000, 0.000000000000000000, 0.000000000000000000 ) ) ;
#10249 = ORIENTED_EDGE ( 'NONE', *, *, #21151, .T. ) ;
#10250 = LINE ( 'NONE', #9834, #14685 ) ;
#10251 = CARTESIAN_POINT ( 'NONE',  ( 3.627054932750481964, 32.93424481021354921, 68.00000000000000000 ) ) ;
#10252 = CARTESIAN_POINT ( 'NONE',  ( -1.774728116533986766, 43.31054587065082728, 37.66679706732590915 ) ) ;
#10253 = VECTOR ( 'NONE', #12063, 1000.000000000000000 ) ;
#10254 = ORIENTED_EDGE ( 'NONE', *, *, #10220, .T. ) ;
#10255 = AXIS2_PLACEMENT_3D ( 'NONE', #14477, #21337, #12804 ) ;
#10256 = CIRCLE ( 'NONE', #20964, 0.5000000000000004441 ) ;
#10257 = ORIENTED_EDGE ( 'NONE', *, *, #2918, .T. ) ;
#10258 = ORIENTED_EDGE ( 'NONE', *, *, #17677, .F. ) ;
#10259 = DIRECTION ( 'NONE',  ( -4.336808689941893885E-15, 0.000000000000000000, 1.000000000000000000 ) ) ;
#10260 = EDGE_CURVE ( 'NONE', #11697, #7044, #2042, .T. ) ;
#10261 = LINE ( 'NONE', #6812, #15357 ) ;
#10262 = EDGE_LOOP ( 'NONE', ( #16732, #16149, #10108, #11963, #4367, #11604, #9921, #4015, #16028, #6663, #14727, #8092, #4280, #15412, #18359, #4356 ) ) ;
#10263 = CARTESIAN_POINT ( 'NONE',  ( 15.95292532278785913, 34.11873716947361856, 68.00000000000000000 ) ) ;
#10264 = AXIS2_PLACEMENT_3D ( 'NONE', #10094, #16902, #15338 ) ;
#10265 = ORIENTED_EDGE ( 'NONE', *, *, #10242, .F. ) ;
#10266 = DIRECTION ( 'NONE',  ( 0.000000000000000000, 1.000000000000000000, 0.000000000000000000 ) ) ;
#10267 = EDGE_LOOP ( 'NONE', ( #16436, #16042, #12046, #15031 ) ) ;
#10268 = LINE ( 'NONE', #3330, #17407 ) ;
#10269 = CIRCLE ( 'NONE', #21043, 5.299999999999998934 ) ;
#10270 = CARTESIAN_POINT ( 'NONE',  ( 23.02398829872513986, -2.157133568460768647, 7.500000000000000000 ) ) ;
#10271 = VECTOR ( 'NONE', #15320, 1000.000000000000000 ) ;
#10272 = CIRCLE ( 'NONE', #597, 0.2999999999999999334 ) ;
#10273 = DIRECTION ( 'NONE',  ( 0.000000000000000000, -0.000000000000000000, -1.000000000000000000 ) ) ;
#10274 = FACE_OUTER_BOUND ( 'NONE', #3647, .T. ) ;
#10275 = VERTEX_POINT ( 'NONE', #7020 ) ;
#10276 = CARTESIAN_POINT ( 'NONE',  ( 23.02398829872513630, 2.558844643944980568, 13.47100117844888167 ) ) ;
#10277 = DIRECTION ( 'NONE',  ( -0.000000000000000000, -1.000000000000000000, -0.000000000000000000 ) ) ;
#10278 = ADVANCED_FACE ( 'NONE', ( #18536 ), #15615, .T. ) ;
#10279 = AXIS2_PLACEMENT_3D ( 'NONE', #13243, #3185, #8111 ) ;
#10280 = FACE_OUTER_BOUND ( 'NONE', #405, .T. ) ;
#10281 = FACE_OUTER_BOUND ( 'NONE', #595, .T. ) ;
#10282 = EDGE_LOOP ( 'NONE', ( #19557, #11255, #1133, #5980 ) ) ;
#10283 = ADVANCED_FACE ( 'NONE', ( #18877 ), #6726, .T. ) ;
#10284 = VECTOR ( 'NONE', #1623, 1000.000000000000000 ) ;
#10285 = CYLINDRICAL_SURFACE ( 'NONE', #16633, 0.2999999999999999334 ) ;
#10286 = ORIENTED_EDGE ( 'NONE', *, *, #13316, .T. ) ;
#10287 = CARTESIAN_POINT ( 'NONE',  ( -14.66174975910705136, -32.10873716947361345, 13.79999999999999893 ) ) ;
#10288 = CARTESIAN_POINT ( 'NONE',  ( 15.95292532278785913, 50.11873716947361856, 13.50000000000000000 ) ) ;
#10289 = CIRCLE ( 'NONE', #2413, 0.2500000000000002220 ) ;
#10290 = CIRCLE ( 'NONE', #4207, 2.299999999999993161 ) ;
#10291 = AXIS2_PLACEMENT_3D ( 'NONE', #7179, #19134, #17778 ) ;
#10292 = ORIENTED_EDGE ( 'NONE', *, *, #21974, .T. ) ;
#10293 = CYLINDRICAL_SURFACE ( 'NONE', #596, 0.04999999999999991257 ) ;
#10294 = AXIS2_PLACEMENT_3D ( 'NONE', #5350, #17288, #18988 ) ;
#10295 = EDGE_LOOP ( 'NONE', ( #10635, #5621, #14611, #6944 ) ) ;
#10296 = ADVANCED_FACE ( 'NONE', ( #18644 ), #8849, .T. ) ;
#10297 = AXIS2_PLACEMENT_3D ( 'NONE', #18721, #20418, #20181 ) ;
#10298 = TOROIDAL_SURFACE ( 'NONE', #17418, 1.000000000000000000, 0.5000000000000000000 ) ;
#10299 = DIRECTION ( 'NONE',  ( 0.000000000000000000, -1.000000000000000000, -0.000000000000000000 ) ) ;
#10300 = VERTEX_POINT ( 'NONE', #16959 ) ;
#10301 = PLANE ( 'NONE',  #21715 ) ;
#10302 = B_SPLINE_CURVE_WITH_KNOTS ( 'NONE', 3,
 ( #18341, #16652, #13411, #1329 ),
 .UNSPECIFIED., .F., .F.,
 ( 4, 4 ),
 ( 0.005071647684206891972, 0.007900577432593609145 ),
 .UNSPECIFIED. ) ;
#10303 = CARTESIAN_POINT ( 'NONE',  ( -19.85144383993102934, 42.46645089659918426, 13.74999999999999822 ) ) ;
#10304 = ADVANCED_FACE ( 'NONE', ( #9929 ), #1522, .F. ) ;
#10305 = DIRECTION ( 'NONE',  ( 0.000000000000000000, 1.000000000000000000, 0.000000000000000000 ) ) ;
#10306 = ADVANCED_FACE ( 'NONE', ( #15167 ), #11809, .T. ) ;
#10307 = TOROIDAL_SURFACE ( 'NONE', #638, 4.700000000000004619, 0.2999999999999999889 ) ;
#10308 = VECTOR ( 'NONE', #1540, 1000.000000000000000 ) ;
#10309 = CARTESIAN_POINT ( 'NONE',  ( 1.824728116533979705, 43.26054587065083012, 33.66679706732590915 ) ) ;
#10310 = DIRECTION ( 'NONE',  ( 0.000000000000000000, -0.000000000000000000, -1.000000000000000000 ) ) ;
#10311 = AXIS2_PLACEMENT_3D ( 'NONE', #12275, #8732, #5825 ) ;
#10312 = DIRECTION ( 'NONE',  ( -0.000000000000000000, -0.000000000000000000, -1.000000000000000000 ) ) ;
#10313 = VECTOR ( 'NONE', #16009, 1000.000000000000000 ) ;
#10314 = CIRCLE ( 'NONE', #17098, 0.04999999999999991257 ) ;
#10315 = ORIENTED_EDGE ( 'NONE', *, *, #11543, .F. ) ;
#10316 = FACE_OUTER_BOUND ( 'NONE', #15222, .T. ) ;
#10317 = DIRECTION ( 'NONE',  ( 0.2309407893632113573, -0.9729678061520313781, 0.000000000000000000 ) ) ;
#10318 = CARTESIAN_POINT ( 'NONE',  ( 1.724728116533979616, 43.31054587065082728, 27.80876104995653719 ) ) ;
#10319 = ORIENTED_EDGE ( 'NONE', *, *, #319, .F. ) ;
#10320 = ORIENTED_EDGE ( 'NONE', *, *, #2791, .T. ) ;
#10321 = FACE_OUTER_BOUND ( 'NONE', #7897, .T. ) ;
#10322 = DIRECTION ( 'NONE',  ( 0.000000000000000000, 0.000000000000000000, 1.000000000000000000 ) ) ;
#10323 = EDGE_CURVE ( 'NONE', #12999, #1527, #7431, .T. ) ;
#10324 = ORIENTED_EDGE ( 'NONE', *, *, #14244, .F. ) ;
#10325 = VECTOR ( 'NONE', #21863, 1000.000000000000000 ) ;
#10326 = ORIENTED_EDGE ( 'NONE', *, *, #3915, .F. ) ;
#10327 = AXIS2_PLACEMENT_3D ( 'NONE', #12042, #20568, #21009 ) ;
#10328 = VECTOR ( 'NONE', #9338, 1000.000000000000000 ) ;
#10329 = CIRCLE ( 'NONE', #1008, 3.500000000000003109 ) ;
#10330 = ORIENTED_EDGE ( 'NONE', *, *, #16015, .T. ) ;
#10331 = EDGE_CURVE ( 'NONE', #1345, #10960, #21364, .T. ) ;
#10332 = DIRECTION ( 'NONE',  ( 0.000000000000000000, 0.000000000000000000, -1.000000000000000000 ) ) ;
#10333 = CARTESIAN_POINT ( 'NONE',  ( 14.96512931750545938, -51.87344388792876515, 13.83591901640606459 ) ) ;
#10334 = ADVANCED_FACE ( 'NONE', ( #12239 ), #10994, .T. ) ;
#10335 = CARTESIAN_POINT ( 'NONE',  ( -15.95292532278785913, 52.11873716947361856, 68.50000000000000000 ) ) ;
#10336 = CARTESIAN_POINT ( 'NONE',  ( -34.40000000000001279, 85.00000000000000000, 79.69999999999998863 ) ) ;
#10337 = CARTESIAN_POINT ( 'NONE',  ( 4.127054932750481520, -33.43424481021354921, 68.00000000000000000 ) ) ;
#10338 = CARTESIAN_POINT ( 'NONE',  ( -17.45292532278785913, 34.11873716947361856, 68.50000000000000000 ) ) ;
#10339 = AXIS2_PLACEMENT_3D ( 'NONE', #21012, #5802, #6020 ) ;
#10340 = CARTESIAN_POINT ( 'NONE',  ( 23.04906723162513416, -2.296088124452698942, 13.26119099173120475 ) ) ;
#10341 = CARTESIAN_POINT ( 'NONE',  ( 25.37540678000427263, -68.74634676501045760, 7.200000000000000178 ) ) ;
#10342 = FACE_OUTER_BOUND ( 'NONE', #17496, .T. ) ;
#10343 = EDGE_LOOP ( 'NONE', ( #3298, #19627, #10831, #21651 ) ) ;
#10344 = ORIENTED_EDGE ( 'NONE', *, *, #5003, .T. ) ;
#10345 = DIRECTION ( 'NONE',  ( 1.000000000000000000, 0.000000000000000000, 0.000000000000000000 ) ) ;
#10346 = VECTOR ( 'NONE', #10949, 1000.000000000000000 ) ;
#10347 = FILL_AREA_STYLE_COLOUR ( '', #14059 ) ;
#10348 = DIRECTION ( 'NONE',  ( 1.000000000000000000, 0.000000000000000000, 0.000000000000000000 ) ) ;
#10349 = EDGE_CURVE ( 'NONE', #398, #4495, #9118, .T. ) ;
#10350 = ORIENTED_EDGE ( 'NONE', *, *, #14872, .F. ) ;
#10351 = CARTESIAN_POINT ( 'NONE',  ( -15.95292532278785913, 50.11873716947361856, 68.00000000000000000 ) ) ;
#10352 = CARTESIAN_POINT ( 'NONE',  ( -31.44597781366221412, 27.99124249474150972, 70.25000000000000000 ) ) ;
#10353 = ADVANCED_FACE ( 'NONE', ( #607 ), #19312, .T. ) ;
#10354 = CARTESIAN_POINT ( 'NONE',  ( -25.37540678000427263, 63.74634676501045050, 13.50000000000000000 ) ) ;
#10355 =( GEOMETRIC_REPRESENTATION_CONTEXT ( 3 ) GLOBAL_UNCERTAINTY_ASSIGNED_CONTEXT ( ( #1235 ) ) GLOBAL_UNIT_ASSIGNED_CONTEXT ( ( #13754, #20276, #6972 ) ) REPRESENTATION_CONTEXT ( 'NONE', 'WORKASPACE' ) );
#10356 = VECTOR ( 'NONE', #17224, 1000.000000000000000 ) ;
#10357 = ADVANCED_FACE ( 'NONE', ( #10701 ), #3990, .T. ) ;
#10358 = DIRECTION ( 'NONE',  ( -0.000000000000000000, -0.000000000000000000, -1.000000000000000000 ) ) ;
#10359 = ORIENTED_EDGE ( 'NONE', *, *, #14138, .F. ) ;
#10360 = CARTESIAN_POINT ( 'NONE',  ( -28.57540678000427548, -63.74634676501045050, 13.50000000000000000 ) ) ;
#10361 = ADVANCED_FACE ( 'NONE', ( #2290 ), #2072, .F. ) ;
#10362 = CARTESIAN_POINT ( 'NONE',  ( 0.000000000000000000, 38.74634676501045760, 42.50000000000000000 ) ) ;
#10363 = DIRECTION ( 'NONE',  ( 2.832483164223434527E-16, -1.000000000000000000, -0.000000000000000000 ) ) ;
#10364 = CARTESIAN_POINT ( 'NONE',  ( 1.724728116533979616, 43.31054587065082728, 53.76679706732590347 ) ) ;
#10365 = DIRECTION ( 'NONE',  ( -0.000000000000000000, -0.000000000000000000, -1.000000000000000000 ) ) ;
#10366 = CARTESIAN_POINT ( 'NONE',  ( 29.13662752439705272, -4.700000000000000178, 3.500000000000000000 ) ) ;
#10367 = VERTEX_POINT ( 'NONE', #7462 ) ;
#10368 = DIRECTION ( 'NONE',  ( 1.000000000000000000, 0.000000000000000000, 0.000000000000000000 ) ) ;
#10369 = DIRECTION ( 'NONE',  ( 1.000000000000000000, 0.000000000000000000, 0.000000000000000000 ) ) ;
#10370 = DIRECTION ( 'NONE',  ( 0.000000000000000000, 0.000000000000000000, 1.000000000000000000 ) ) ;
#10371 = ORIENTED_EDGE ( 'NONE', *, *, #13781, .F. ) ;
#10372 = ORIENTED_EDGE ( 'NONE', *, *, #16885, .F. ) ;
#10373 = VERTEX_POINT ( 'NONE', #20671 ) ;
#10374 = DIRECTION ( 'NONE',  ( 0.000000000000000000, -1.000000000000000000, 0.000000000000000000 ) ) ;
#10375 = DIRECTION ( 'NONE',  ( 4.336808689942043768E-15, 0.000000000000000000, 1.000000000000000000 ) ) ;
#10376 = LINE ( 'NONE', #17184, #4086 ) ;
#10377 = VECTOR ( 'NONE', #17765, 1000.000000000000000 ) ;
#10378 = CIRCLE ( 'NONE', #4277, 1.000000000000000888 ) ;
#10379 = CIRCLE ( 'NONE', #14285, 0.05000000000000143219 ) ;
#10380 = ADVANCED_FACE ( 'NONE', ( #281 ), #14261, .F. ) ;
#10381 = ORIENTED_EDGE ( 'NONE', *, *, #21406, .F. ) ;
#10382 = DIRECTION ( 'NONE',  ( 0.000000000000000000, 0.000000000000000000, -1.000000000000000000 ) ) ;
#10383 = ORIENTED_EDGE ( 'NONE', *, *, #10854, .T. ) ;
#10384 = CARTESIAN_POINT ( 'NONE',  ( 1.774728116533979660, 42.31054587065082728, 45.66679706732590205 ) ) ;
#10385 = DIRECTION ( 'NONE',  ( 0.000000000000000000, 0.000000000000000000, 1.000000000000000000 ) ) ;
#10386 = DIRECTION ( 'NONE',  ( 0.000000000000000000, 1.000000000000000000, 0.000000000000000000 ) ) ;
#10387 = CARTESIAN_POINT ( 'NONE',  ( -10.22290649399594997, 43.00645089659918341, 68.06527860057354928 ) ) ;
#10388 = ORIENTED_EDGE ( 'NONE', *, *, #16800, .T. ) ;
#10389 = CARTESIAN_POINT ( 'NONE',  ( 23.02398829872513986, 3.528912754968628551, 13.80000000000000071 ) ) ;
#10390 = ADVANCED_FACE ( 'NONE', ( #13930 ), #4087, .T. ) ;
#10391 = DIRECTION ( 'NONE',  ( -0.000000000000000000, -0.000000000000000000, -1.000000000000000000 ) ) ;
#10392 = CIRCLE ( 'NONE', #5751, 0.2999999999999999334 ) ;
#10393 = AXIS2_PLACEMENT_3D ( 'NONE', #1732, #3194, #15381 ) ;
#10394 = CARTESIAN_POINT ( 'NONE',  ( -25.37540678000427263, -67.54634676501045476, 7.500000000000000000 ) ) ;
#10395 = PRODUCT_DEFINITION_SHAPE ( 'NONE', 'NONE',  #4251 ) ;
#10396 = DIRECTION ( 'NONE',  ( 0.000000000000000000, 0.000000000000000000, -1.000000000000000000 ) ) ;
#10397 = EDGE_LOOP ( 'NONE', ( #14077, #6347, #3781 ) ) ;
#10398 = PRESENTATION_STYLE_ASSIGNMENT (( #21132 ) ) ;
#10399 = DIRECTION ( 'NONE',  ( -0.000000000000000000, 0.000000000000000000, 1.000000000000000000 ) ) ;
#10400 = ORIENTED_EDGE ( 'NONE', *, *, #9038, .F. ) ;
#10401 = FACE_OUTER_BOUND ( 'NONE', #981, .T. ) ;
#10402 = ORIENTED_EDGE ( 'NONE', *, *, #19839, .F. ) ;
#10403 = ORIENTED_EDGE ( 'NONE', *, *, #21645, .T. ) ;
#10404 = DIRECTION ( 'NONE',  ( -1.000000000000000000, 0.000000000000000000, 0.000000000000000000 ) ) ;
#10405 = CIRCLE ( 'NONE', #730, 0.05000000000000143219 ) ;
#10406 = EDGE_CURVE ( 'NONE', #6840, #8641, #13829, .T. ) ;
#10407 = AXIS2_PLACEMENT_3D ( 'NONE', #2248, #2140, #3835 ) ;
#10408 = VERTEX_POINT ( 'NONE', #19091 ) ;
#10409 = ADVANCED_FACE ( 'NONE', ( #3758, #15601 ), #9022, .T. ) ;
#10410 = VERTEX_POINT ( 'NONE', #10580 ) ;
#10411 = DIRECTION ( 'NONE',  ( -2.388292521039847891E-16, 0.000000000000000000, -1.000000000000000000 ) ) ;
#10412 = DIRECTION ( 'NONE',  ( -1.000000000000000000, 0.000000000000000000, 0.000000000000000000 ) ) ;
#10413 = B_SPLINE_CURVE_WITH_KNOTS ( 'NONE', 3,
 ( #8067, #19941, #1118, #21731 ),
 .UNSPECIFIED., .F., .F.,
 ( 4, 4 ),
 ( 0.001759598111914162421, 0.004588913574811922039 ),
 .UNSPECIFIED. ) ;
#10414 = VECTOR ( 'NONE', #20872, 1000.000000000000000 ) ;
#10415 = CARTESIAN_POINT ( 'NONE',  ( -9.178906393579158163, 42.46645089659918426, 68.06527860057354928 ) ) ;
#10416 = LINE ( 'NONE', #208, #6429 ) ;
#10417 = FACE_OUTER_BOUND ( 'NONE', #8278, .T. ) ;
#10418 = ADVANCED_FACE ( 'NONE', ( #10480 ), #2421, .T. ) ;
#10419 = ORIENTED_EDGE ( 'NONE', *, *, #14300, .F. ) ;
#10420 = CARTESIAN_POINT ( 'NONE',  ( 3.627054932750481964, 33.43424481021354921, 7.321391277662001151 ) ) ;
#10421 = CYLINDRICAL_SURFACE ( 'NONE', #21722, 2.500000000000002220 ) ;
#10422 = CIRCLE ( 'NONE', #7215, 4.351418481279137218 ) ;
#10423 = CARTESIAN_POINT ( 'NONE',  ( 26.37540678000427619, -10.94079601157914716, 42.50000000000000000 ) ) ;
#10424 = AXIS2_PLACEMENT_3D ( 'NONE', #17021, #12505, #3925 ) ;
#10425 = ORIENTED_EDGE ( 'NONE', *, *, #20169, .F. ) ;
#10426 = EDGE_LOOP ( 'NONE', ( #2796, #16122, #5937, #20184 ) ) ;
#10427 = DIRECTION ( 'NONE',  ( 0.000000000000000000, 0.000000000000000000, 1.000000000000000000 ) ) ;
#10428 = PRODUCT_CONTEXT ( 'NONE', #8020, 'mechanical' ) ;
#10429 = EDGE_CURVE ( 'NONE', #3082, #10879, #4197, .T. ) ;
#10430 = VECTOR ( 'NONE', #3052, 1000.000000000000000 ) ;
#10431 = VERTEX_POINT ( 'NONE', #20883 ) ;
#10432 = VECTOR ( 'NONE', #1850, 1000.000000000000000 ) ;
#10433 = ORIENTED_EDGE ( 'NONE', *, *, #7050, .T. ) ;
#10434 = ORIENTED_EDGE ( 'NONE', *, *, #11870, .F. ) ;
#10435 = CARTESIAN_POINT ( 'NONE',  ( -31.01761816434227015, 84.00847499568689614, 13.75000000000000000 ) ) ;
#10436 = CARTESIAN_POINT ( 'NONE',  ( 4.127054932750481520, 33.43424481021354921, 68.00000000000000000 ) ) ;
#10437 = VECTOR ( 'NONE', #7675, 1000.000000000000000 ) ;
#10438 = DIRECTION ( 'NONE',  ( -1.000000000000000000, 0.000000000000000000, 0.000000000000000000 ) ) ;
#10439 = ADVANCED_FACE ( 'NONE', ( #3881 ), #18175, .F. ) ;
#10440 = VECTOR ( 'NONE', #17907, 1000.000000000000000 ) ;
#10441 = CARTESIAN_POINT ( 'NONE',  ( -23.02398829872513630, 2.211005313989852894, 13.25071573983079887 ) ) ;
#10442 = CIRCLE ( 'NONE', #5808, 0.5000000000000004441 ) ;
#10443 = AXIS2_PLACEMENT_3D ( 'NONE', #18952, #4969, #241 ) ;
#10444 = DIRECTION ( 'NONE',  ( 0.000000000000000000, -1.000000000000000000, 0.000000000000000000 ) ) ;
#10445 = CARTESIAN_POINT ( 'NONE',  ( 23.11756190325309035, -2.646657027129584172, 13.40142076604335841 ) ) ;
#10446 = DIRECTION ( 'NONE',  ( 1.000000000000000000, 0.000000000000000000, 0.000000000000000000 ) ) ;
#10447 = CIRCLE ( 'NONE', #5458, 0.04999999999999991257 ) ;
#10448 = DIRECTION ( 'NONE',  ( -0.000000000000000000, -1.000000000000000000, -0.000000000000000000 ) ) ;
#10449 = ORIENTED_EDGE ( 'NONE', *, *, #14882, .T. ) ;
#10450 = ORIENTED_EDGE ( 'NONE', *, *, #20262, .F. ) ;
#10451 = DIRECTION ( 'NONE',  ( -0.9729678061520402599, -0.2309407893631745812, -0.000000000000000000 ) ) ;
#10452 = EDGE_CURVE ( 'NONE', #15418, #5793, #12794, .T. ) ;
#10453 = CARTESIAN_POINT ( 'NONE',  ( -1.824728116533986810, 43.26054587065083012, 35.80876104995653009 ) ) ;
#10454 = ORIENTED_EDGE ( 'NONE', *, *, #17908, .T. ) ;
#10455 = EDGE_CURVE ( 'NONE', #12289, #17196, #21010, .T. ) ;
#10456 = CIRCLE ( 'NONE', #8315, 1.826718556943725202 ) ;
#10457 = AXIS2_PLACEMENT_3D ( 'NONE', #976, #2998, #18094 ) ;
#10458 = CARTESIAN_POINT ( 'NONE',  ( 14.66174975910705847, 0.000000000000000000, 13.50000000000000000 ) ) ;
#10459 = CARTESIAN_POINT ( 'NONE',  ( 32.20000000000001705, 71.00000000000001421, 3.200000000000000178 ) ) ;
#10460 = DIRECTION ( 'NONE',  ( 0.000000000000000000, 0.000000000000000000, -1.000000000000000000 ) ) ;
#10461 = ORIENTED_EDGE ( 'NONE', *, *, #10854, .F. ) ;
#10462 = DIRECTION ( 'NONE',  ( -0.000000000000000000, -1.000000000000000000, 0.000000000000000000 ) ) ;
#10463 = AXIS2_PLACEMENT_3D ( 'NONE', #3504, #20513, #1481 ) ;
#10464 = CARTESIAN_POINT ( 'NONE',  ( 0.000000000000000000, -67.54634676501045476, 7.799999999999999822 ) ) ;
#10465 = EDGE_CURVE ( 'NONE', #10522, #16645, #15274, .T. ) ;
#10466 = DIRECTION ( 'NONE',  ( 0.000000000000000000, 0.000000000000000000, -1.000000000000000000 ) ) ;
#10467 = DIRECTION ( 'NONE',  ( 0.000000000000000000, 0.000000000000000000, 1.000000000000000000 ) ) ;
#10468 = CARTESIAN_POINT ( 'NONE',  ( -3.127054932750481964, -32.11873716947361856, 68.50000000000000000 ) ) ;
#10469 = CARTESIAN_POINT ( 'NONE',  ( -4.127054932750482408, -32.93424481021354921, 68.50000000000000000 ) ) ;
#10470 = CYLINDRICAL_SURFACE ( 'NONE', #5418, 0.1000000000000028644 ) ;
#10471 = FACE_OUTER_BOUND ( 'NONE', #18678, .T. ) ;
#10472 = CARTESIAN_POINT ( 'NONE',  ( 1.724728116533979838, 42.31054587065082728, 33.66679706732590915 ) ) ;
#10473 = VERTEX_POINT ( 'NONE', #21326 ) ;
#10474 = ORIENTED_EDGE ( 'NONE', *, *, #1887, .F. ) ;
#10475 = ORIENTED_EDGE ( 'NONE', *, *, #20339, .F. ) ;
#10476 = CARTESIAN_POINT ( 'NONE',  ( -30.79999999999999361, -84.70000000000001705, 0.3000000000000002665 ) ) ;
#10477 = CARTESIAN_POINT ( 'NONE',  ( -8.638906393579159015, 43.34579957953053508, 69.00503344894293889 ) ) ;
#10478 = EDGE_CURVE ( 'NONE', #12714, #16486, #13131, .T. ) ;
#10479 = EDGE_CURVE ( 'NONE', #416, #5585, #9689, .T. ) ;
#10480 = FACE_OUTER_BOUND ( 'NONE', #21988, .T. ) ;
#10481 = EDGE_CURVE ( 'NONE', #20437, #21381, #14367, .T. ) ;
#10482 = ORIENTED_EDGE ( 'NONE', *, *, #6134, .T. ) ;
#10483 = CARTESIAN_POINT ( 'NONE',  ( 0.000000000000000000, 85.00000000000000000, 0.000000000000000000 ) ) ;
#10484 = ORIENTED_EDGE ( 'NONE', *, *, #8286, .F. ) ;
#10485 = DIRECTION ( 'NONE',  ( -0.000000000000000000, -1.000000000000000000, -0.000000000000000000 ) ) ;
#10486 = DIRECTION ( 'NONE',  ( -0.000000000000000000, 1.000000000000000000, -0.000000000000000000 ) ) ;
#10487 = FACE_OUTER_BOUND ( 'NONE', #20812, .T. ) ;
#10488 = DIRECTION ( 'NONE',  ( -8.673617379884034239E-17, 0.000000000000000000, 1.000000000000000000 ) ) ;
#10489 = ORIENTED_EDGE ( 'NONE', *, *, #601, .T. ) ;
#10490 = DIRECTION ( 'NONE',  ( -0.000000000000000000, -0.000000000000000000, -1.000000000000000000 ) ) ;
#10491 = DIRECTION ( 'NONE',  ( 0.000000000000000000, 0.000000000000000000, 1.000000000000000000 ) ) ;
#10492 = ADVANCED_FACE ( 'NONE', ( #19986 ), #8503, .T. ) ;
#10493 = CARTESIAN_POINT ( 'NONE',  ( 0.000000000000000000, -52.10286008774954780, 13.87500000000000000 ) ) ;
#10494 = LINE ( 'NONE', #15308, #16387 ) ;
#10495 = EDGE_LOOP ( 'NONE', ( #5278, #15186, #2344, #5677 ) ) ;
#10496 = DIRECTION ( 'NONE',  ( -1.224646799147353207E-16, 0.000000000000000000, -1.000000000000000000 ) ) ;
#10497 = VERTEX_POINT ( 'NONE', #2963 ) ;
#10498 = CARTESIAN_POINT ( 'NONE',  ( -1.774728116533986544, 43.26054587065083012, 31.80876104995653719 ) ) ;
#10499 = MECHANICAL_DESIGN_GEOMETRIC_PRESENTATION_REPRESENTATION (  '', ( #20515 ), #15842 ) ;
#10500 = ORIENTED_EDGE ( 'NONE', *, *, #19585, .T. ) ;
#10501 = DIRECTION ( 'NONE',  ( 0.000000000000000000, 0.000000000000000000, 1.000000000000000000 ) ) ;
#10502 = DIRECTION ( 'NONE',  ( -1.000000000000000000, 0.000000000000000000, 0.000000000000000000 ) ) ;
#10503 = EDGE_LOOP ( 'NONE', ( #19224, #19656, #19083, #1238 ) ) ;
#10504 = EDGE_CURVE ( 'NONE', #14287, #21506, #13071, .T. ) ;
#10505 = ORIENTED_EDGE ( 'NONE', *, *, #12215, .T. ) ;
#10506 = EDGE_CURVE ( 'NONE', #20211, #15626, #6002, .T. ) ;
#10507 = VECTOR ( 'NONE', #12586, 1000.000000000000000 ) ;
#10508 = ORIENTED_EDGE ( 'NONE', *, *, #21797, .F. ) ;
#10509 = ORIENTED_EDGE ( 'NONE', *, *, #20142, .T. ) ;
#10510 = DIRECTION ( 'NONE',  ( 1.000000000000000000, 0.000000000000000000, 0.000000000000000000 ) ) ;
#10511 = CIRCLE ( 'NONE', #20882, 0.2999999999999999889 ) ;
#10512 = FACE_OUTER_BOUND ( 'NONE', #1620, .T. ) ;
#10513 = CARTESIAN_POINT ( 'NONE',  ( -15.95292532278785913, 50.11873716947361856, 68.50000000000000000 ) ) ;
#10514 = DIRECTION ( 'NONE',  ( 1.000000000000000000, 0.000000000000000000, 0.000000000000000000 ) ) ;
#10515 = UNCERTAINTY_MEASURE_WITH_UNIT (LENGTH_MEASURE( 1.000000000000000082E-05 ), #8855, 'distance_accuracy_value', 'NONE');
#10516 = ORIENTED_EDGE ( 'NONE', *, *, #15131, .F. ) ;
#10517 = CARTESIAN_POINT ( 'NONE',  ( -9.141460742840918030, -32.93424481021354921, 68.00000000000000000 ) ) ;
#10518 = EDGE_CURVE ( 'NONE', #17549, #15658, #3447, .T. ) ;
#10519 = DIRECTION ( 'NONE',  ( 0.000000000000000000, 0.000000000000000000, 1.000000000000000000 ) ) ;
#10520 = ADVANCED_FACE ( 'NONE', ( #2857 ), #9341, .T. ) ;
#10521 = CARTESIAN_POINT ( 'NONE',  ( 9.641460742840918030, -32.11873716947361856, 68.00000000000000000 ) ) ;
#10522 = VERTEX_POINT ( 'NONE', #16148 ) ;
#10523 = CARTESIAN_POINT ( 'NONE',  ( 34.39999999999998437, 84.70000000000001705, 0.3000000000000042077 ) ) ;
#10524 = CARTESIAN_POINT ( 'NONE',  ( -14.96174975910705207, 51.76873716947361714, 13.50000000000000000 ) ) ;
#10525 = EDGE_LOOP ( 'NONE', ( #2389, #8306, #11925, #11177 ) ) ;
#10526 = ORIENTED_EDGE ( 'NONE', *, *, #12682, .F. ) ;
#10527 = CARTESIAN_POINT ( 'NONE',  ( 0.000000000000000000, 0.000000000000000000, 139.0000000000000000 ) ) ;
#10528 = VERTEX_POINT ( 'NONE', #4412 ) ;
#10529 = CARTESIAN_POINT ( 'NONE',  ( 23.02398829872514341, -3.297363125858362665, 13.54387027667928933 ) ) ;
#10530 = ORIENTED_EDGE ( 'NONE', *, *, #17726, .T. ) ;
#10531 = VERTEX_POINT ( 'NONE', #14465 ) ;
#10532 = DIRECTION ( 'NONE',  ( 2.388292521039847891E-16, 0.000000000000000000, 1.000000000000000000 ) ) ;
#10533 = CARTESIAN_POINT ( 'NONE',  ( 30.37540678000427619, -63.74634676501045050, 7.500000000000000000 ) ) ;
#10534 = DIRECTION ( 'NONE',  ( 0.000000000000000000, 0.000000000000000000, -1.000000000000000000 ) ) ;
#10535 = AXIS2_PLACEMENT_3D ( 'NONE', #15948, #7485, #14284 ) ;
#10536 = DIRECTION ( 'NONE',  ( 0.000000000000000000, 0.000000000000000000, 1.000000000000000000 ) ) ;
#10537 = AXIS2_PLACEMENT_3D ( 'NONE', #13768, #32, #15787 ) ;
#10538 = PRESENTATION_STYLE_ASSIGNMENT (( #234 ) ) ;
#10539 = CARTESIAN_POINT ( 'NONE',  ( -23.02398829872514341, 2.558598175897728755, 13.47089014135852736 ) ) ;
#10540 = DIRECTION ( 'NONE',  ( -1.000000000000000000, 0.000000000000000000, -8.673617379883930701E-17 ) ) ;
#10541 = ADVANCED_FACE ( 'NONE', ( #7786 ), #19637, .F. ) ;
#10542 = DIRECTION ( 'NONE',  ( -1.000000000000000000, 0.000000000000000000, 0.000000000000000000 ) ) ;
#10543 = CYLINDRICAL_SURFACE ( 'NONE', #14631, 0.2999999999999999334 ) ;
#10544 = CARTESIAN_POINT ( 'NONE',  ( -25.37540678000427263, -68.74634676501045760, 7.500000000000000000 ) ) ;
#10545 = DIRECTION ( 'NONE',  ( 1.000000000000000000, 3.387630566026860322E-15, -1.224646799147353207E-16 ) ) ;
#10546 = ORIENTED_EDGE ( 'NONE', *, *, #20532, .T. ) ;
#10547 = VERTEX_POINT ( 'NONE', #16588 ) ;
#10548 = LINE ( 'NONE', #8988, #21753 ) ;
#10549 = CARTESIAN_POINT ( 'NONE',  ( -33.50000000000000000, 85.00000000000000000, 1.800000000000000266 ) ) ;
#10550 = VERTEX_POINT ( 'NONE', #9448 ) ;
#10551 = AXIS2_PLACEMENT_3D ( 'NONE', #9466, #11041, #7922 ) ;
#10552 = VECTOR ( 'NONE', #6350, 1000.000000000000000 ) ;
#10553 = ADVANCED_FACE ( 'NONE', ( #14590 ), #7568, .T. ) ;
#10554 = DIRECTION ( 'NONE',  ( 1.000000000000000000, 0.000000000000000000, -2.388292521039847891E-16 ) ) ;
#10555 = CARTESIAN_POINT ( 'NONE',  ( 28.87540678000427619, 63.74634676501045050, 13.50000000000000000 ) ) ;
#10556 = AXIS2_PLACEMENT_3D ( 'NONE', #20543, #11476, #2979 ) ;
#10557 = VERTEX_POINT ( 'NONE', #21220 ) ;
#10558 = PLANE ( 'NONE',  #13215 ) ;
#10559 = DIRECTION ( 'NONE',  ( 0.000000000000000000, 0.000000000000000000, 1.000000000000000000 ) ) ;
#10560 = EDGE_CURVE ( 'NONE', #3514, #2571, #10579, .T. ) ;
#10561 = CARTESIAN_POINT ( 'NONE',  ( -15.21174975910705207, -41.81054587065082728, 68.25000000000000000 ) ) ;
#10562 = CARTESIAN_POINT ( 'NONE',  ( -27.37540678000427974, -10.94079601157914716, 42.50000000000000000 ) ) ;
#10563 = CARTESIAN_POINT ( 'NONE',  ( 0.000000000000000000, 67.24634676501045760, 13.50000000000000000 ) ) ;
#10564 = DIRECTION ( 'NONE',  ( -0.000000000000000000, -1.000000000000000000, -0.000000000000000000 ) ) ;
#10565 = VECTOR ( 'NONE', #2018, 1000.000000000000000 ) ;
#10566 = AXIS2_PLACEMENT_3D ( 'NONE', #21791, #22126, #17065 ) ;
#10567 = AXIS2_PLACEMENT_3D ( 'NONE', #4903, #13714, #8483 ) ;
#10568 = VERTEX_POINT ( 'NONE', #12669 ) ;
#10569 = DIRECTION ( 'NONE',  ( 1.000000000000000000, 0.000000000000000000, 0.000000000000000000 ) ) ;
#10570 = CARTESIAN_POINT ( 'NONE',  ( 1.824728116533979261, 43.31054587065082728, 43.70876104995653577 ) ) ;
#10571 = DIRECTION ( 'NONE',  ( -0.000000000000000000, 0.000000000000000000, 1.000000000000000000 ) ) ;
#10572 = ORIENTED_EDGE ( 'NONE', *, *, #680, .F. ) ;
#10573 = VERTEX_POINT ( 'NONE', #934 ) ;
#10574 = ORIENTED_EDGE ( 'NONE', *, *, #14438, .F. ) ;
#10575 = DIRECTION ( 'NONE',  ( 0.000000000000000000, -1.000000000000000000, -0.000000000000000000 ) ) ;
#10576 = DIRECTION ( 'NONE',  ( -0.000000000000000000, -1.000000000000000000, -0.000000000000000000 ) ) ;
#10577 = LINE ( 'NONE', #5349, #12485 ) ;
#10578 = VECTOR ( 'NONE', #16212, 1000.000000000000000 ) ;
#10579 = CIRCLE ( 'NONE', #9507, 0.05000000000000143219 ) ;
#10580 = CARTESIAN_POINT ( 'NONE',  ( 23.02398829872514341, -5.683640910026986681, 42.50000000000000000 ) ) ;
#10581 = VECTOR ( 'NONE', #1697, 1000.000000000000000 ) ;
#10582 = ADVANCED_FACE ( 'NONE', ( #11891 ), #22035, .F. ) ;
#10583 = ORIENTED_EDGE ( 'NONE', *, *, #5488, .F. ) ;
#10584 = DIRECTION ( 'NONE',  ( 0.000000000000000000, -0.000000000000000000, 1.000000000000000000 ) ) ;
#10585 = VECTOR ( 'NONE', #4710, 1000.000000000000000 ) ;
#10586 = AXIS2_PLACEMENT_3D ( 'NONE', #367, #7113, #5767 ) ;
#10587 = ORIENTED_EDGE ( 'NONE', *, *, #2972, .F. ) ;
#10588 = CARTESIAN_POINT ( 'NONE',  ( -28.79994065384636315, -6.566898051583388352, 13.40260211333369256 ) ) ;
#10589 = CARTESIAN_POINT ( 'NONE',  ( -1.774728116533986766, 43.26054587065083012, 41.66679706732590915 ) ) ;
#10590 = DIRECTION ( 'NONE',  ( 0.000000000000000000, -1.000000000000000000, 0.000000000000000000 ) ) ;
#10591 = LINE ( 'NONE', #5571, #10224 ) ;
#10592 = EDGE_LOOP ( 'NONE', ( #20988, #16907, #14943, #8132 ) ) ;
#10593 = CARTESIAN_POINT ( 'NONE',  ( 23.04273156199908712, 2.261510999193106386, 13.20000000000004015 ) ) ;
#10594 = DIRECTION ( 'NONE',  ( 0.000000000000000000, 1.000000000000000000, 0.000000000000000000 ) ) ;
#10595 = ADVANCED_FACE ( 'NONE', ( #3295 ), #11998, .T. ) ;
#10596 = ADVANCED_FACE ( 'NONE', ( #11781 ), #15040, .T. ) ;
#10597 = DIRECTION ( 'NONE',  ( -1.000000000000000000, 0.000000000000000000, 0.000000000000000000 ) ) ;
#10598 = DIRECTION ( 'NONE',  ( -8.673617379884034239E-17, 0.000000000000000000, 1.000000000000000000 ) ) ;
#10599 = ORIENTED_EDGE ( 'NONE', *, *, #8254, .F. ) ;
#10600 = AXIS2_PLACEMENT_3D ( 'NONE', #7912, #20196, #13144 ) ;
#10601 = AXIS2_PLACEMENT_3D ( 'NONE', #20006, #21903, #4882 ) ;
#10602 = PLANE ( 'NONE',  #18401 ) ;
#10603 = CIRCLE ( 'NONE', #12365, 0.2999999999999999334 ) ;
#10604 = EDGE_CURVE ( 'NONE', #17808, #630, #9864, .T. ) ;
#10605 = ORIENTED_EDGE ( 'NONE', *, *, #15120, .F. ) ;
#10606 = DIRECTION ( 'NONE',  ( 0.000000000000000000, -1.000000000000000000, 0.000000000000000000 ) ) ;
#10607 = ORIENTED_EDGE ( 'NONE', *, *, #12703, .F. ) ;
#10608 = AXIS2_PLACEMENT_3D ( 'NONE', #20058, #20391, #16558 ) ;
#10609 = ORIENTED_EDGE ( 'NONE', *, *, #1298, .F. ) ;
#10610 = LINE ( 'NONE', #7046, #1379 ) ;
#10611 = DIRECTION ( 'NONE',  ( -0.000000000000000000, 0.000000000000000000, 1.000000000000000000 ) ) ;
#10612 = ORIENTED_EDGE ( 'NONE', *, *, #4959, .F. ) ;
#10613 = EDGE_CURVE ( 'NONE', #21066, #7220, #14864, .T. ) ;
#10614 = EDGE_LOOP ( 'NONE', ( #12611, #10371, #4559, #16869 ) ) ;
#10615 = AXIS2_PLACEMENT_3D ( 'NONE', #4761, #11563, #6566 ) ;
#10616 = VECTOR ( 'NONE', #19510, 1000.000000000000000 ) ;
#10617 = VECTOR ( 'NONE', #2661, 1000.000000000000000 ) ;
#10618 = ORIENTED_EDGE ( 'NONE', *, *, #15261, .F. ) ;
#10619 = LINE ( 'NONE', #12603, #3138 ) ;
#10620 = AXIS2_PLACEMENT_3D ( 'NONE', #13746, #7595, #10317 ) ;
#10621 = CARTESIAN_POINT ( 'NONE',  ( 30.07540678000427548, 63.74634676501045050, 7.200000000000000178 ) ) ;
#10622 = CARTESIAN_POINT ( 'NONE',  ( 3.627054932750481964, 32.61873716947361856, 68.50000000000000000 ) ) ;
#10623 = EDGE_CURVE ( 'NONE', #3486, #19413, #13770, .T. ) ;
#10624 = DIRECTION ( 'NONE',  ( 1.000000000000000000, -0.000000000000000000, 0.000000000000000000 ) ) ;
#10625 = ORIENTED_EDGE ( 'NONE', *, *, #14015, .F. ) ;
#10626 = DIRECTION ( 'NONE',  ( -1.000000000000000000, 0.000000000000000000, 0.000000000000000000 ) ) ;
#10627 = EDGE_CURVE ( 'NONE', #18406, #17937, #6119, .T. ) ;
#10628 = CARTESIAN_POINT ( 'NONE',  ( -1.724728116533986721, 42.31054587065082728, 27.80876104995653719 ) ) ;
#10629 = CARTESIAN_POINT ( 'NONE',  ( -9.178906393579158163, 42.46645089659918426, 67.75164986378473486 ) ) ;
#10630 = TOROIDAL_SURFACE ( 'NONE', #19207, 1.500000000000000000, 0.5000000000000000000 ) ;
#10631 = VECTOR ( 'NONE', #12953, 1000.000000000000000 ) ;
#10632 = ORIENTED_EDGE ( 'NONE', *, *, #8738, .F. ) ;
#10633 = DIRECTION ( 'NONE',  ( -0.000000000000000000, 1.000000000000000000, 0.000000000000000000 ) ) ;
#10634 = PLANE ( 'NONE',  #962 ) ;
#10635 = ORIENTED_EDGE ( 'NONE', *, *, #21277, .T. ) ;
#10636 = ORIENTED_EDGE ( 'NONE', *, *, #7013, .T. ) ;
#10637 = CIRCLE ( 'NONE', #4922, 0.3000000000000016542 ) ;
#10638 = CARTESIAN_POINT ( 'NONE',  ( -25.37540678000426908, 38.74634676501045760, 13.79999999999999893 ) ) ;
#10639 = CIRCLE ( 'NONE', #12750, 5.193574995607837863 ) ;
#10640 = CONTEXT_DEPENDENT_SHAPE_REPRESENTATION ( #21034, #18387 ) ;
#10641 = ORIENTED_EDGE ( 'NONE', *, *, #15476, .F. ) ;
#10642 = ADVANCED_FACE ( 'NONE', ( #20422 ), #11631, .T. ) ;
#10643 = CARTESIAN_POINT ( 'NONE',  ( 23.04273156199908357, -2.261510999192897220, 13.19999999999999218 ) ) ;
#10644 = ORIENTED_EDGE ( 'NONE', *, *, #18025, .T. ) ;
#10645 = CLOSED_SHELL ( 'NONE', ( #16063, #18600, #10390, #2388, #19742, #15420, #6842, #7492, #17490, #13006, #4205, #16248, #21264, #14822, #21904, #11810, #19130, #13194, #18146, #448, #6080, #10582, #14986, #2341, #21233, #9790, #3745, #10074, #12525, #2842, #5918, #11107 ) ) ;
#10646 = AXIS2_PLACEMENT_3D ( 'NONE', #9453, #6458, #18181 ) ;
#10647 = AXIS2_PLACEMENT_3D ( 'NONE', #18079, #6253, #2987 ) ;
#10648 = ORIENTED_EDGE ( 'NONE', *, *, #16305, .F. ) ;
#10649 = LINE ( 'NONE', #9075, #10565 ) ;
#10650 = CARTESIAN_POINT ( 'NONE',  ( -24.00488095381848197, 42.46645089659918426, 68.50000000000000000 ) ) ;
#10651 = PLANE ( 'NONE',  #1287 ) ;
#10652 = VECTOR ( 'NONE', #5722, 1000.000000000000000 ) ;
#10653 = AXIS2_PLACEMENT_3D ( 'NONE', #12432, #3731, #10777 ) ;
#10654 = FACE_OUTER_BOUND ( 'NONE', #17573, .T. ) ;
#10655 = AXIS2_PLACEMENT_3D ( 'NONE', #15174, #6823, #17406 ) ;
#10656 = EDGE_CURVE ( 'NONE', #11890, #20195, #10012, .T. ) ;
#10657 = CARTESIAN_POINT ( 'NONE',  ( -23.04897344237150492, 2.295898177910673965, 13.26544997878583487 ) ) ;
#10658 = FACE_OUTER_BOUND ( 'NONE', #4030, .T. ) ;
#10659 = DIRECTION ( 'NONE',  ( 0.000000000000000000, -1.000000000000000000, 0.000000000000000000 ) ) ;
#10660 = CARTESIAN_POINT ( 'NONE',  ( -21.92816239687475743, 42.46645089659918426, 68.50000000000000000 ) ) ;
#10661 = CARTESIAN_POINT ( 'NONE',  ( 1.724728116533979616, 42.36054587065083155, 33.76679706732591058 ) ) ;
#10662 = AXIS2_PLACEMENT_3D ( 'NONE', #12986, #19616, #21420 ) ;
#10663 = VECTOR ( 'NONE', #1700, 1000.000000000000000 ) ;
#10664 = ORIENTED_EDGE ( 'NONE', *, *, #11376, .T. ) ;
#10665 = EDGE_LOOP ( 'NONE', ( #8112, #14056, #12551, #2677, #20649, #8465, #11488, #2428 ) ) ;
#10666 = LINE ( 'NONE', #17482, #16710 ) ;
#10667 = DIRECTION ( 'NONE',  ( 0.000000000000000000, -1.000000000000000000, 0.000000000000000000 ) ) ;
#10668 = TOROIDAL_SURFACE ( 'NONE', #18165, 4.051418481279135619, 0.2999999999999999889 ) ;
#10669 = ORIENTED_EDGE ( 'NONE', *, *, #16599, .F. ) ;
#10670 = AXIS2_PLACEMENT_3D ( 'NONE', #2618, #18173, #17833 ) ;
#10671 = CARTESIAN_POINT ( 'NONE',  ( 3.127054932750481964, 33.43424481021354921, 68.50000000000000000 ) ) ;
#10672 = AXIS2_PLACEMENT_3D ( 'NONE', #1807, #4827, #21855 ) ;
#10673 = ORIENTED_EDGE ( 'NONE', *, *, #8101, .F. ) ;
#10674 = CIRCLE ( 'NONE', #12094, 0.3000000000000003775 ) ;
#10675 = EDGE_CURVE ( 'NONE', #6635, #5485, #12692, .T. ) ;
#10676 = ADVANCED_FACE ( 'NONE', ( #6450 ), #17046, .F. ) ;
#10677 = CARTESIAN_POINT ( 'NONE',  ( -23.02398829872513986, 5.683640910026983128, 42.50000000000000000 ) ) ;
#10678 = AXIS2_PLACEMENT_3D ( 'NONE', #6601, #18097, #13396 ) ;
#10679 = DIRECTION ( 'NONE',  ( -1.000000000000000000, 0.000000000000000000, 0.000000000000000000 ) ) ;
#10680 = VERTEX_POINT ( 'NONE', #20091 ) ;
#10681 = DIRECTION ( 'NONE',  ( -1.000000000000000000, 0.000000000000000000, 0.000000000000000000 ) ) ;
#10682 = CARTESIAN_POINT ( 'NONE',  ( -1.824728116533986810, 42.36054587065083155, 33.66679706732590915 ) ) ;
#10683 = DIRECTION ( 'NONE',  ( -1.000000000000000000, -0.000000000000000000, -0.000000000000000000 ) ) ;
#10684 = CIRCLE ( 'NONE', #14974, 0.05000000000000143219 ) ;
#10685 = FACE_OUTER_BOUND ( 'NONE', #7235, .T. ) ;
#10686 = CYLINDRICAL_SURFACE ( 'NONE', #14702, 0.05000000000000143219 ) ;
#10687 = PLANE ( 'NONE',  #8069 ) ;
#10688 = LINE ( 'NONE', #17910, #18827 ) ;
#10689 = CIRCLE ( 'NONE', #13542, 1.750000000000001554 ) ;
#10690 = CARTESIAN_POINT ( 'NONE',  ( -29.17540678000427690, -63.74634676501045050, 7.500000000000000000 ) ) ;
#10691 = DIRECTION ( 'NONE',  ( 1.000000000000000000, 0.000000000000000000, 0.000000000000000000 ) ) ;
#10692 = DIRECTION ( 'NONE',  ( 0.000000000000000000, 1.000000000000000000, 0.000000000000000000 ) ) ;
#10693 = EDGE_CURVE ( 'NONE', #8671, #4102, #8560, .T. ) ;
#10694 = ORIENTED_EDGE ( 'NONE', *, *, #13731, .F. ) ;
#10695 = EDGE_LOOP ( 'NONE', ( #12403, #6806, #21853, #2582 ) ) ;
#10696 = ORIENTED_EDGE ( 'NONE', *, *, #15184, .T. ) ;
#10697 = CARTESIAN_POINT ( 'NONE',  ( -29.01868551570922605, -6.499165645473476971, 7.532495484408729958 ) ) ;
#10698 = CARTESIAN_POINT ( 'NONE',  ( -8.638906393579159015, 43.49585613540820361, 70.88527860057354246 ) ) ;
#10699 = DIRECTION ( 'NONE',  ( 0.000000000000000000, 0.000000000000000000, 1.000000000000000000 ) ) ;
#10700 = EDGE_LOOP ( 'NONE', ( #5578, #21412, #8592, #19530 ) ) ;
#10701 = FACE_OUTER_BOUND ( 'NONE', #4756, .T. ) ;
#10702 = EDGE_CURVE ( 'NONE', #12570, #16460, #16820, .T. ) ;
#10703 = CIRCLE ( 'NONE', #687, 0.2500000000000002220 ) ;
#10704 = VERTEX_POINT ( 'NONE', #13349 ) ;
#10705 = CARTESIAN_POINT ( 'NONE',  ( 31.50000000000002132, -72.00000000000001421, 1.800000000000000044 ) ) ;
#10706 = DIRECTION ( 'NONE',  ( -0.000000000000000000, -0.000000000000000000, -1.000000000000000000 ) ) ;
#10707 = ORIENTED_EDGE ( 'NONE', *, *, #16127, .T. ) ;
#10708 = CARTESIAN_POINT ( 'NONE',  ( -28.87540678000427619, -6.494748934539263274, 13.19999999999999929 ) ) ;
#10709 = DIRECTION ( 'NONE',  ( 0.000000000000000000, 0.000000000000000000, 1.000000000000000000 ) ) ;
#10710 = CARTESIAN_POINT ( 'NONE',  ( 17.45292532278785913, 0.000000000000000000, 68.00000000000000000 ) ) ;
#10711 = DIRECTION ( 'NONE',  ( 0.000000000000000000, 0.000000000000000000, 1.000000000000000000 ) ) ;
#10712 = ORIENTED_EDGE ( 'NONE', *, *, #3066, .T. ) ;
#10713 = DIRECTION ( 'NONE',  ( 1.000000000000000000, 0.000000000000000000, -0.000000000000000000 ) ) ;
#10714 = CARTESIAN_POINT ( 'NONE',  ( 23.04273156199908357, -2.261510999192741345, 13.50000000000000000 ) ) ;
#10715 = LINE ( 'NONE', #10493, #14066 ) ;
#10716 = DIRECTION ( 'NONE',  ( -0.000000000000000000, 1.000000000000000000, 0.000000000000000000 ) ) ;
#10717 = ORIENTED_EDGE ( 'NONE', *, *, #18340, .F. ) ;
#10718 = CIRCLE ( 'NONE', #19289, 1.299999999999999156 ) ;
#10719 = EDGE_CURVE ( 'NONE', #20520, #15862, #910, .T. ) ;
#10720 = EDGE_LOOP ( 'NONE', ( #20057, #14953, #12379, #14309 ) ) ;
#10721 = AXIS2_PLACEMENT_3D ( 'NONE', #3439, #8155, #1305 ) ;
#10722 = STYLED_ITEM ( 'NONE', ( #5173 ), #7548 ) ;
#10723 = DIRECTION ( 'NONE',  ( 0.000000000000000000, -1.000000000000000000, 0.000000000000000000 ) ) ;
#10724 = VECTOR ( 'NONE', #8590, 1000.000000000000000 ) ;
#10725 = PLANE ( 'NONE',  #8080 ) ;
#10726 = ORIENTED_EDGE ( 'NONE', *, *, #20453, .T. ) ;
#10727 = ORIENTED_EDGE ( 'NONE', *, *, #5701, .T. ) ;
#10728 = CARTESIAN_POINT ( 'NONE',  ( -21.92816239687475743, 42.46645089659918426, 13.74999999999999822 ) ) ;
#10729 = VERTEX_POINT ( 'NONE', #18846 ) ;
#10730 = EDGE_CURVE ( 'NONE', #4642, #627, #6896, .T. ) ;
#10731 = EDGE_CURVE ( 'NONE', #2970, #10879, #3187, .T. ) ;
#10732 = ADVANCED_FACE ( 'NONE', ( #12312 ), #13902, .F. ) ;
#10733 = ORIENTED_EDGE ( 'NONE', *, *, #19340, .T. ) ;
#10734 = AXIS2_PLACEMENT_3D ( 'NONE', #20219, #3100, #16746 ) ;
#10735 = ORIENTED_EDGE ( 'NONE', *, *, #7078, .T. ) ;
#10736 = CARTESIAN_POINT ( 'NONE',  ( 27.37540678000426908, 36.74634676501047181, 42.50000000000000000 ) ) ;
#10737 = AXIS2_PLACEMENT_3D ( 'NONE', #19295, #19071, #2163 ) ;
#10738 = DIRECTION ( 'NONE',  ( 0.000000000000000000, 0.000000000000000000, -1.000000000000000000 ) ) ;
#10739 = CARTESIAN_POINT ( 'NONE',  ( 28.87540678000427619, 6.494748934539263274, 7.720760502796167657 ) ) ;
#10740 = CARTESIAN_POINT ( 'NONE',  ( 34.39999999999998437, -84.70000000000001705, 0.6000000000000041966 ) ) ;
#10741 = VERTEX_POINT ( 'NONE', #3236 ) ;
#10742 = DIRECTION ( 'NONE',  ( 0.000000000000000000, 0.000000000000000000, 1.000000000000000000 ) ) ;
#10743 = ADVANCED_FACE ( 'NONE', ( #8613 ), #10285, .T. ) ;
#10744 = FACE_OUTER_BOUND ( 'NONE', #20881, .T. ) ;
#10745 = CARTESIAN_POINT ( 'NONE',  ( 15.21174975910705918, 52.39333383871510108, 13.50000000000000000 ) ) ;
#10746 = AXIS2_PLACEMENT_3D ( 'NONE', #3299, #20308, #4861 ) ;
#10747 = ORIENTED_EDGE ( 'NONE', *, *, #19901, .F. ) ;
#10748 = CARTESIAN_POINT ( 'NONE',  ( 30.67540678000428045, 0.000000000000000000, 3.799999999999999822 ) ) ;
#10749 = AXIS2_PLACEMENT_3D ( 'NONE', #1479, #8546, #8656 ) ;
#10750 = EDGE_LOOP ( 'NONE', ( #21095, #16509, #4880, #6477 ) ) ;
#10751 = VERTEX_POINT ( 'NONE', #11601 ) ;
#10752 = DIRECTION ( 'NONE',  ( 0.000000000000000000, -1.000000000000000000, 0.000000000000000000 ) ) ;
#10753 = ADVANCED_FACE ( 'NONE', ( #20361 ), #16872, .T. ) ;
#10754 = ORIENTED_EDGE ( 'NONE', *, *, #17869, .T. ) ;
#10755 = EDGE_CURVE ( 'NONE', #15401, #14671, #10165, .T. ) ;
#10756 = ORIENTED_EDGE ( 'NONE', *, *, #6493, .T. ) ;
#10757 = EDGE_CURVE ( 'NONE', #6609, #7001, #1775, .T. ) ;
#10758 = CARTESIAN_POINT ( 'NONE',  ( 23.02398829872514341, -2.192121262983568908, 13.33089993820311925 ) ) ;
#10759 = ORIENTED_EDGE ( 'NONE', *, *, #19380, .F. ) ;
#10760 = ORIENTED_EDGE ( 'NONE', *, *, #6310, .F. ) ;
#10761 = CARTESIAN_POINT ( 'NONE',  ( 1.724728116533979616, 43.26054587065083012, 31.80876104995653719 ) ) ;
#10762 = DIRECTION ( 'NONE',  ( 0.000000000000000000, 0.000000000000000000, -1.000000000000000000 ) ) ;
#10763 = CYLINDRICAL_SURFACE ( 'NONE', #5204, 0.3000000000000016542 ) ;
#10764 = DIRECTION ( 'NONE',  ( -0.000000000000000000, 0.000000000000000000, 1.000000000000000000 ) ) ;
#10765 = VECTOR ( 'NONE', #13040, 1000.000000000000000 ) ;
#10766 = CARTESIAN_POINT ( 'NONE',  ( -1.824728116533986810, 43.31054587065082728, 41.76679706732590347 ) ) ;
#10767 = EDGE_CURVE ( 'NONE', #9267, #4383, #4911, .T. ) ;
#10768 = DIRECTION ( 'NONE',  ( 0.000000000000000000, 1.000000000000000000, -0.000000000000000000 ) ) ;
#10769 = DIRECTION ( 'NONE',  ( 0.000000000000000000, 1.000000000000000000, 0.000000000000000000 ) ) ;
#10770 = PLANE ( 'NONE',  #5553 ) ;
#10771 = FACE_BOUND ( 'NONE', #7949, .T. ) ;
#10772 = ADVANCED_FACE ( 'NONE', ( #1650 ), #11723, .F. ) ;
#10773 = CIRCLE ( 'NONE', #435, 0.04999999999999991257 ) ;
#10774 = VECTOR ( 'NONE', #12782, 1000.000000000000000 ) ;
#10775 = ORIENTED_EDGE ( 'NONE', *, *, #1363, .F. ) ;
#10776 = ORIENTED_EDGE ( 'NONE', *, *, #2250, .F. ) ;
#10777 = DIRECTION ( 'NONE',  ( 0.000000000000000000, 0.000000000000000000, 1.000000000000000000 ) ) ;
#10778 = DIRECTION ( 'NONE',  ( 0.000000000000000000, 0.000000000000000000, 1.000000000000000000 ) ) ;
#10779 = ORIENTED_EDGE ( 'NONE', *, *, #5723, .T. ) ;
#10780 = EDGE_LOOP ( 'NONE', ( #494, #11885, #7073, #18153 ) ) ;
#10781 = ORIENTED_EDGE ( 'NONE', *, *, #14677, .F. ) ;
#10782 = EDGE_CURVE ( 'NONE', #1460, #857, #6716, .T. ) ;
#10783 = AXIS2_PLACEMENT_3D ( 'NONE', #11213, #18034, #6437 ) ;
#10784 = CIRCLE ( 'NONE', #20799, 2.000000000000000000 ) ;
#10785 = DIRECTION ( 'NONE',  ( 1.000000000000000000, 0.000000000000000000, 0.000000000000000000 ) ) ;
#10786 = AXIS2_PLACEMENT_3D ( 'NONE', #3288, #13454, #1824 ) ;
#10787 = CARTESIAN_POINT ( 'NONE',  ( -33.50000000000000000, 84.70000000000001705, 1.800000000000000266 ) ) ;
#10788 = ORIENTED_EDGE ( 'NONE', *, *, #15782, .F. ) ;
#10789 = CARTESIAN_POINT ( 'NONE',  ( 3.127054932750481964, 32.11873716947361856, 68.00000000000000000 ) ) ;
#10790 = DIRECTION ( 'NONE',  ( 0.000000000000000000, 0.000000000000000000, -1.000000000000000000 ) ) ;
#10791 = DIRECTION ( 'NONE',  ( 1.000000000000000000, 0.000000000000000000, 0.000000000000000000 ) ) ;
#10792 = CARTESIAN_POINT ( 'NONE',  ( -8.641460742840918030, 32.93424481021354921, 68.50000000000000000 ) ) ;
#10793 = CARTESIAN_POINT ( 'NONE',  ( -1.724728116533986721, 42.36054587065083155, 47.80876104995653719 ) ) ;
#10794 = CARTESIAN_POINT ( 'NONE',  ( -1.724728116533986721, 43.31054587065082728, 33.66679706732590915 ) ) ;
#10795 = EDGE_CURVE ( 'NONE', #19115, #1830, #13723, .T. ) ;
#10796 = CARTESIAN_POINT ( 'NONE',  ( -18.91037735075775217, 42.46645089659918426, 68.50000000000000000 ) ) ;
#10797 = FACE_OUTER_BOUND ( 'NONE', #9671, .T. ) ;
#10798 = EDGE_CURVE ( 'NONE', #19790, #9336, #21303, .T. ) ;
#10799 = CARTESIAN_POINT ( 'NONE',  ( 30.79999999999999361, 85.00000000000000000, 4.029087969194791265E-15 ) ) ;
#10800 = EDGE_CURVE ( 'NONE', #8248, #6058, #5137, .T. ) ;
#10801 = ORIENTED_EDGE ( 'NONE', *, *, #9675, .F. ) ;
#10802 = ORIENTED_EDGE ( 'NONE', *, *, #5124, .F. ) ;
#10803 = ORIENTED_EDGE ( 'NONE', *, *, #3463, .F. ) ;
#10804 = DIRECTION ( 'NONE',  ( 1.000000000000000000, 0.000000000000000000, 0.000000000000000000 ) ) ;
#10805 = AXIS2_PLACEMENT_3D ( 'NONE', #17587, #237, #3838 ) ;
#10806 = DIRECTION ( 'NONE',  ( 1.000000000000000000, 0.000000000000000000, 0.000000000000000000 ) ) ;
#10807 = TOROIDAL_SURFACE ( 'NONE', #2220, 3.800000000000002931, 0.2999999999999999889 ) ;
#10808 = DIRECTION ( 'NONE',  ( 0.000000000000000000, 1.000000000000000000, 0.000000000000000000 ) ) ;
#10809 = ORIENTED_EDGE ( 'NONE', *, *, #7736, .T. ) ;
#10810 = DIRECTION ( 'NONE',  ( -1.000000000000000000, 0.000000000000000000, 0.000000000000000000 ) ) ;
#10811 = LINE ( 'NONE', #3581, #4520 ) ;
#10812 = VERTEX_POINT ( 'NONE', #18331 ) ;
#10813 = DIRECTION ( 'NONE',  ( -2.388292521039847891E-16, 0.000000000000000000, -1.000000000000000000 ) ) ;
#10814 = DIRECTION ( 'NONE',  ( -1.000000000000000000, -0.000000000000000000, -0.000000000000000000 ) ) ;
#10815 = LINE ( 'NONE', #396, #15718 ) ;
#10816 = DIRECTION ( 'NONE',  ( 1.000000000000000000, 0.000000000000000000, -0.000000000000000000 ) ) ;
#10817 = ORIENTED_EDGE ( 'NONE', *, *, #16178, .F. ) ;
#10818 = PLANE ( 'NONE',  #11283 ) ;
#10819 = FACE_OUTER_BOUND ( 'NONE', #14264, .T. ) ;
#10820 = DIRECTION ( 'NONE',  ( 0.000000000000000000, 0.000000000000000000, 1.000000000000000000 ) ) ;
#10821 = CARTESIAN_POINT ( 'NONE',  ( -23.04692967985607055, -2.284552260428336368, 13.25236378595243103 ) ) ;
#10822 = ORIENTED_EDGE ( 'NONE', *, *, #1108, .F. ) ;
#10823 = DIRECTION ( 'NONE',  ( -6.123233995736764803E-17, 0.000000000000000000, 1.000000000000000000 ) ) ;
#10824 = EDGE_CURVE ( 'NONE', #12787, #4126, #11940, .T. ) ;
#10825 = ORIENTED_EDGE ( 'NONE', *, *, #21718, .T. ) ;
#10826 = LINE ( 'NONE', #409, #18764 ) ;
#10827 = EDGE_CURVE ( 'NONE', #11459, #1254, #9835, .T. ) ;
#10828 = ORIENTED_EDGE ( 'NONE', *, *, #3092, .F. ) ;
#10829 = EDGE_LOOP ( 'NONE', ( #2879, #2551, #7560, #9762 ) ) ;
#10830 = DIRECTION ( 'NONE',  ( -1.000000000000000000, 0.000000000000000000, 0.000000000000000000 ) ) ;
#10831 = ORIENTED_EDGE ( 'NONE', *, *, #4647, .F. ) ;
#10832 = ORIENTED_EDGE ( 'NONE', *, *, #10504, .T. ) ;
#10833 = EDGE_LOOP ( 'NONE', ( #5782, #6422, #14132, #16607 ) ) ;
#10834 = DIRECTION ( 'NONE',  ( -0.000000000000000000, -0.000000000000000000, -1.000000000000000000 ) ) ;
#10835 = DIRECTION ( 'NONE',  ( 0.000000000000000000, 0.000000000000000000, 1.000000000000000000 ) ) ;
#10836 = CARTESIAN_POINT ( 'NONE',  ( 1.774728116533973665, 42.31054587065082728, 16.00000000000000000 ) ) ;
#10837 = DIRECTION ( 'NONE',  ( 1.000000000000000000, 0.000000000000000000, 0.000000000000000000 ) ) ;
#10838 = PLANE ( 'NONE',  #12545 ) ;
#10839 = ORIENTED_EDGE ( 'NONE', *, *, #18523, .F. ) ;
#10840 = SHAPE_REPRESENTATION ( 'Cross Recess Screw', ( #17493 ), #3707 ) ;
#10841 = LINE ( 'NONE', #5498, #22160 ) ;
#10842 = EDGE_CURVE ( 'NONE', #823, #20557, #17723, .T. ) ;
#10843 = DIRECTION ( 'NONE',  ( 0.000000000000000000, 0.000000000000000000, 1.000000000000000000 ) ) ;
#10844 = LINE ( 'NONE', #15861, #19033 ) ;
#10845 = ORIENTED_EDGE ( 'NONE', *, *, #8719, .T. ) ;
#10846 = DIRECTION ( 'NONE',  ( -6.123233995736764803E-17, 0.000000000000000000, 1.000000000000000000 ) ) ;
#10847 = ORIENTED_EDGE ( 'NONE', *, *, #9505, .T. ) ;
#10848 = EDGE_LOOP ( 'NONE', ( #12685, #13126, #13149, #15961 ) ) ;
#10849 = ORIENTED_EDGE ( 'NONE', *, *, #8563, .F. ) ;
#10850 = CARTESIAN_POINT ( 'NONE',  ( 29.37540678000427619, -5.000000000000000000, 7.200000000000000178 ) ) ;
#10851 = ORIENTED_EDGE ( 'NONE', *, *, #21239, .T. ) ;
#10852 = EDGE_LOOP ( 'NONE', ( #688, #21881, #9812, #4871 ) ) ;
#10853 = COLOUR_RGB ( '', 0.66274510, 0.83137255, 0.94901961) ;
#10854 = EDGE_CURVE ( 'NONE', #7338, #11408, #7262, .T. ) ;
#10855 = CARTESIAN_POINT ( 'NONE',  ( 23.07499583180669589, -2.433548416302916628, 13.33575415462846081 ) ) ;
#10856 = ORIENTED_EDGE ( 'NONE', *, *, #12421, .F. ) ;
#10857 = CARTESIAN_POINT ( 'NONE',  ( 23.32398829872514057, 2.157133568460765538, 13.19999999999999929 ) ) ;
#10858 = ORIENTED_EDGE ( 'NONE', *, *, #17758, .F. ) ;
#10859 = CARTESIAN_POINT ( 'NONE',  ( -1.774728116533986766, 43.26054587065083012, 16.00000000000000000 ) ) ;
#10860 = CYLINDRICAL_SURFACE ( 'NONE', #14506, 0.2999999999999999334 ) ;
#10861 = VECTOR ( 'NONE', #181, 1000.000000000000000 ) ;
#10862 = DIRECTION ( 'NONE',  ( 3.052134192567367925E-16, -1.000000000000000000, 0.000000000000000000 ) ) ;
#10863 = DIRECTION ( 'NONE',  ( 0.000000000000000000, -1.000000000000000000, 0.000000000000000000 ) ) ;
#10864 = ADVANCED_FACE ( 'NONE', ( #8935 ), #17421, .F. ) ;
#10865 = EDGE_CURVE ( 'NONE', #13985, #5446, #19886, .T. ) ;
#10866 = CARTESIAN_POINT ( 'NONE',  ( -23.02398829872513986, 2.279831973701412107, 13.43058255391197697 ) ) ;
#10867 = AXIS2_PLACEMENT_3D ( 'NONE', #18348, #6622, #9973 ) ;
#10868 = EDGE_CURVE ( 'NONE', #6809, #11011, #7487, .T. ) ;
#10869 = CARTESIAN_POINT ( 'NONE',  ( 0.000000000000000000, 32.61873716947361856, 68.00000000000000000 ) ) ;
#10870 = AXIS2_PLACEMENT_3D ( 'NONE', #6970, #17013, #3705 ) ;
#10871 = LINE ( 'NONE', #17909, #20912 ) ;
#10872 = PLANE ( 'NONE',  #13242 ) ;
#10873 = VECTOR ( 'NONE', #17500, 1000.000000000000000 ) ;
#10874 = EDGE_CURVE ( 'NONE', #12853, #5745, #17638, .T. ) ;
#10875 = DIRECTION ( 'NONE',  ( -1.000000000000000000, 0.000000000000000000, 0.000000000000000000 ) ) ;
#10876 = ORIENTED_EDGE ( 'NONE', *, *, #14540, .F. ) ;
#10877 = CARTESIAN_POINT ( 'NONE',  ( 3.627054932750481520, 32.93424481021354921, 42.50000000000000000 ) ) ;
#10878 = EDGE_LOOP ( 'NONE', ( #3493, #8404, #798, #13372 ) ) ;
#10879 = VERTEX_POINT ( 'NONE', #4013 ) ;
#10880 = ADVANCED_FACE ( 'NONE', ( #14286 ), #10725, .F. ) ;
#10881 = CIRCLE ( 'NONE', #8042, 0.1000000000000028644 ) ;
#10882 = DIRECTION ( 'NONE',  ( 0.000000000000000000, 0.000000000000000000, 1.000000000000000000 ) ) ;
#10883 = CARTESIAN_POINT ( 'NONE',  ( -9.141460742840918030, -32.61873716947361856, 7.321391277662001151 ) ) ;
#10884 = ORIENTED_EDGE ( 'NONE', *, *, #7546, .F. ) ;
#10885 = CARTESIAN_POINT ( 'NONE',  ( -34.39999999999999858, 84.70000000000001705, 3.673940397442079220E-17 ) ) ;
#10886 = LINE ( 'NONE', #7966, #20013 ) ;
#10887 = LINE ( 'NONE', #12554, #17906 ) ;
#10888 = ADVANCED_FACE ( 'NONE', ( #15739 ), #20591, .T. ) ;
#10889 = CARTESIAN_POINT ( 'NONE',  ( 14.75227361498200551, 52.14371094787964722, 13.50000000000000000 ) ) ;
#10890 = DIRECTION ( 'NONE',  ( 0.000000000000000000, 0.000000000000000000, -1.000000000000000000 ) ) ;
#10891 = CYLINDRICAL_SURFACE ( 'NONE', #6303, 0.05000000000000143219 ) ;
#10892 = EDGE_CURVE ( 'NONE', #21431, #13921, #19226, .T. ) ;
#10893 = CARTESIAN_POINT ( 'NONE',  ( 30.79999999999999716, -84.70000000000001705, 4.029087969194791265E-15 ) ) ;
#10894 = DIRECTION ( 'NONE',  ( 0.000000000000000000, 0.000000000000000000, 1.000000000000000000 ) ) ;
#10895 = CARTESIAN_POINT ( 'NONE',  ( 4.127054932750481520, -32.93424481021354921, 68.50000000000000000 ) ) ;
#10896 = ORIENTED_EDGE ( 'NONE', *, *, #21637, .F. ) ;
#10897 = AXIS2_PLACEMENT_3D ( 'NONE', #9366, #2756, #7687 ) ;
#10898 = ORIENTED_EDGE ( 'NONE', *, *, #7913, .F. ) ;
#10899 = DIRECTION ( 'NONE',  ( -2.107255972849994642E-16, 0.000000000000000000, -1.000000000000000000 ) ) ;
#10900 = CARTESIAN_POINT ( 'NONE',  ( -1.824728116533986810, 43.26054587065083012, 31.80876104995653719 ) ) ;
#10901 = ORIENTED_EDGE ( 'NONE', *, *, #21271, .F. ) ;
#10902 = DIRECTION ( 'NONE',  ( 0.000000000000000000, 0.000000000000000000, 1.000000000000000000 ) ) ;
#10903 = ORIENTED_EDGE ( 'NONE', *, *, #1382, .T. ) ;
#10904 = CARTESIAN_POINT ( 'NONE',  ( 8.641460742840918030, -32.93424481021354921, 68.00000000000000000 ) ) ;
#10905 = SURFACE_STYLE_FILL_AREA ( #18003 ) ;
#10906 = AXIS2_PLACEMENT_3D ( 'NONE', #11937, #6835, #3340 ) ;
#10907 = DIRECTION ( 'NONE',  ( -1.000000000000000000, 0.000000000000000000, 0.000000000000000000 ) ) ;
#10908 = EDGE_CURVE ( 'NONE', #10231, #19849, #20606, .T. ) ;
#10909 = CARTESIAN_POINT ( 'NONE',  ( -28.87540678000428329, -6.494748934539265051, 13.24746166461178554 ) ) ;
#10910 = EDGE_CURVE ( 'NONE', #10367, #15658, #411, .T. ) ;
#10911 = LINE ( 'NONE', #9126, #7458 ) ;
#10912 = VECTOR ( 'NONE', #6136, 1000.000000000000000 ) ;
#10913 = DIRECTION ( 'NONE',  ( 1.000000000000000000, 0.000000000000000000, -2.388292521039847891E-16 ) ) ;
#10914 = VECTOR ( 'NONE', #4992, 1000.000000000000000 ) ;
#10915 = DIRECTION ( 'NONE',  ( 0.000000000000000000, 0.000000000000000000, 1.000000000000000000 ) ) ;
#10916 = AXIS2_PLACEMENT_3D ( 'NONE', #20565, #20227, #12039 ) ;
#10917 = ORIENTED_EDGE ( 'NONE', *, *, #14187, .F. ) ;
#10918 = DIRECTION ( 'NONE',  ( 1.000000000000000000, 0.000000000000000000, 0.000000000000000000 ) ) ;
#10919 = CARTESIAN_POINT ( 'NONE',  ( 1.724728116533979838, 42.36054587065083155, 45.71679706732591342 ) ) ;
#10920 = FACE_OUTER_BOUND ( 'NONE', #21654, .T. ) ;
#10921 = CARTESIAN_POINT ( 'NONE',  ( -1.774728116533986544, 43.26054587065083012, 35.80876104995653009 ) ) ;
#10922 = ORIENTED_EDGE ( 'NONE', *, *, #11896, .F. ) ;
#10923 = FACE_OUTER_BOUND ( 'NONE', #4733, .T. ) ;
#10924 = EDGE_CURVE ( 'NONE', #10145, #1897, #2314, .T. ) ;
#10925 = EDGE_LOOP ( 'NONE', ( #19441, #3912, #16202, #1576 ) ) ;
#10926 = DIRECTION ( 'NONE',  ( 0.000000000000000000, 0.000000000000000000, 1.000000000000000000 ) ) ;
#10927 = DIRECTION ( 'NONE',  ( 0.000000000000000000, 0.000000000000000000, 1.000000000000000000 ) ) ;
#10928 = ORIENTED_EDGE ( 'NONE', *, *, #19560, .F. ) ;
#10929 = AXIS2_PLACEMENT_3D ( 'NONE', #13464, #21985, #18616 ) ;
#10930 = ORIENTED_EDGE ( 'NONE', *, *, #6370, .T. ) ;
#10931 = DIRECTION ( 'NONE',  ( 0.000000000000000000, 0.000000000000000000, 1.000000000000000000 ) ) ;
#10932 = DIRECTION ( 'NONE',  ( 0.000000000000000000, 0.000000000000000000, 1.000000000000000000 ) ) ;
#10933 = ORIENTED_EDGE ( 'NONE', *, *, #21964, .T. ) ;
#10934 = EDGE_LOOP ( 'NONE', ( #7707, #7624, #21981, #22044 ) ) ;
#10935 = ADVANCED_FACE ( 'NONE', ( #13950 ), #9141, .T. ) ;
#10936 = EDGE_LOOP ( 'NONE', ( #2832, #848, #15138, #13791 ) ) ;
#10937 = EDGE_CURVE ( 'NONE', #7824, #3013, #15841, .T. ) ;
#10938 = CIRCLE ( 'NONE', #15213, 2.500000000000002220 ) ;
#10939 = AXIS2_PLACEMENT_3D ( 'NONE', #19544, #4225, #11042 ) ;
#10940 = DIRECTION ( 'NONE',  ( -0.000000000000000000, 1.000000000000000000, -0.000000000000000000 ) ) ;
#10941 = AXIS2_PLACEMENT_3D ( 'NONE', #15201, #21942, #20378 ) ;
#10942 = DIRECTION ( 'NONE',  ( 0.000000000000000000, 0.000000000000000000, -1.000000000000000000 ) ) ;
#10943 = FACE_OUTER_BOUND ( 'NONE', #6035, .T. ) ;
#10944 = DIRECTION ( 'NONE',  ( 0.000000000000000000, 0.000000000000000000, 1.000000000000000000 ) ) ;
#10945 = DIRECTION ( 'NONE',  ( 0.000000000000000000, 0.000000000000000000, 1.000000000000000000 ) ) ;
#10946 = ORIENTED_EDGE ( 'NONE', *, *, #16324, .F. ) ;
#10947 = DIRECTION ( 'NONE',  ( 1.000000000000000000, 0.000000000000000000, 0.000000000000000000 ) ) ;
#10948 = AXIS2_PLACEMENT_3D ( 'NONE', #19732, #14568, #6096 ) ;
#10949 = DIRECTION ( 'NONE',  ( -0.000000000000000000, -1.000000000000000000, 0.000000000000000000 ) ) ;
#10950 = CARTESIAN_POINT ( 'NONE',  ( -1.824728116533986810, 42.36054587065083155, 31.75876104995653648 ) ) ;
#10951 = ORIENTED_EDGE ( 'NONE', *, *, #21581, .T. ) ;
#10952 = CARTESIAN_POINT ( 'NONE',  ( -4.127054932750482408, 32.93424481021354921, 42.50000000000000000 ) ) ;
#10953 = VERTEX_POINT ( 'NONE', #8720 ) ;
#10954 = CIRCLE ( 'NONE', #575, 2.500000000000002220 ) ;
#10955 = ADVANCED_FACE ( 'NONE', ( #14166 ), #8821, .F. ) ;
#10956 = AXIS2_PLACEMENT_3D ( 'NONE', #8777, #10129, #18625 ) ;
#10957 = VECTOR ( 'NONE', #11910, 1000.000000000000000 ) ;
#10958 = ORIENTED_EDGE ( 'NONE', *, *, #17306, .T. ) ;
#10959 = CIRCLE ( 'NONE', #10556, 0.2999999999999947153 ) ;
#10960 = VERTEX_POINT ( 'NONE', #12258 ) ;
#10961 = LINE ( 'NONE', #14760, #251 ) ;
#10962 = ORIENTED_EDGE ( 'NONE', *, *, #21069, .F. ) ;
#10963 = VERTEX_POINT ( 'NONE', #19110 ) ;
#10964 = VECTOR ( 'NONE', #1899, 1000.000000000000000 ) ;
#10965 = ADVANCED_FACE ( 'NONE', ( #18899 ), #4522, .T. ) ;
#10966 = EDGE_CURVE ( 'NONE', #1412, #9063, #17024, .T. ) ;
#10967 = CARTESIAN_POINT ( 'NONE',  ( -21.92816239687475743, 42.46645089659918426, 68.50000000000000000 ) ) ;
#10968 = ORIENTED_EDGE ( 'NONE', *, *, #7023, .T. ) ;
#10969 = CARTESIAN_POINT ( 'NONE',  ( 29.13662752439705272, 0.000000000000000000, 3.799999999999999822 ) ) ;
#10970 = CARTESIAN_POINT ( 'NONE',  ( -9.178906393579161715, 42.46645089659918426, 61.53912392244307483 ) ) ;
#10971 = LINE ( 'NONE', #14534, #3429 ) ;
#10972 = DIRECTION ( 'NONE',  ( 0.000000000000000000, 0.000000000000000000, 1.000000000000000000 ) ) ;
#10973 = AXIS2_PLACEMENT_3D ( 'NONE', #3405, #8677, #21992 ) ;
#10974 = TOROIDAL_SURFACE ( 'NONE', #13822, 1.300000000000000044, 0.2999999999999999889 ) ;
#10975 = AXIS2_PLACEMENT_3D ( 'NONE', #817, #16032, #9333 ) ;
#10976 = CARTESIAN_POINT ( 'NONE',  ( -31.44597781366220701, -6.622080232047910987E-15, 70.25000000000000000 ) ) ;
#10977 = DIRECTION ( 'NONE',  ( 0.000000000000000000, 0.000000000000000000, -1.000000000000000000 ) ) ;
#10978 = AXIS2_PLACEMENT_3D ( 'NONE', #17945, #7902, #4195 ) ;
#10979 = CARTESIAN_POINT ( 'NONE',  ( -35.00000000000000000, -84.70000000000001705, 1.500000000000000000 ) ) ;
#10980 = AXIS2_PLACEMENT_3D ( 'NONE', #7236, #9231, #17831 ) ;
#10981 = EDGE_CURVE ( 'NONE', #4245, #17392, #17861, .T. ) ;
#10982 = DIRECTION ( 'NONE',  ( -0.000000000000000000, -0.000000000000000000, 1.000000000000000000 ) ) ;
#10983 = ORIENTED_EDGE ( 'NONE', *, *, #13195, .F. ) ;
#10984 = ORIENTED_EDGE ( 'NONE', *, *, #12501, .F. ) ;
#10985 = LINE ( 'NONE', #11431, #6023 ) ;
#10986 =( NAMED_UNIT ( * ) SI_UNIT ( $, .STERADIAN. ) SOLID_ANGLE_UNIT ( ) );
#10987 = VECTOR ( 'NONE', #16418, 1000.000000000000000 ) ;
#10988 = AXIS2_PLACEMENT_3D ( 'NONE', #9380, #645, #17763 ) ;
#10989 = VECTOR ( 'NONE', #5935, 1000.000000000000000 ) ;
#10990 = EDGE_LOOP ( 'NONE', ( #5491, #14231, #510, #15030 ) ) ;
#10991 = EDGE_CURVE ( 'NONE', #5643, #18174, #10256, .T. ) ;
#10992 = EDGE_CURVE ( 'NONE', #11808, #13948, #19664, .T. ) ;
#10993 = EDGE_CURVE ( 'NONE', #4678, #20293, #18199, .T. ) ;
#10994 = TOROIDAL_SURFACE ( 'NONE', #21735, 0.05000000000000000278, 0.05000000000000000278 ) ;
#10995 = VECTOR ( 'NONE', #4948, 1000.000000000000000 ) ;
#10996 = CIRCLE ( 'NONE', #21739, 0.2500000000000002220 ) ;
#10997 = FACE_BOUND ( 'NONE', #12541, .T. ) ;
#10998 = CARTESIAN_POINT ( 'NONE',  ( -23.04273156199908357, -2.261510999192741345, 13.50000000000000000 ) ) ;
#10999 = VERTEX_POINT ( 'NONE', #14613 ) ;
#11000 = CARTESIAN_POINT ( 'NONE',  ( 9.641460742840918030, 32.11873716947361856, 68.00000000000000000 ) ) ;
#11001 = DIRECTION ( 'NONE',  ( -1.000000000000000000, 0.000000000000000000, 0.000000000000000000 ) ) ;
#11002 = CARTESIAN_POINT ( 'NONE',  ( 14.71479891986436606, 52.07369784111803312, 13.50000000000000000 ) ) ;
#11003 = DIRECTION ( 'NONE',  ( -1.000000000000000000, 0.000000000000000000, 0.000000000000000000 ) ) ;
#11004 = CIRCLE ( 'NONE', #6012, 0.3000000000000016542 ) ;
#11005 = DIRECTION ( 'NONE',  ( 1.000000000000000000, 0.000000000000000000, 0.000000000000000000 ) ) ;
#11006 = EDGE_CURVE ( 'NONE', #11511, #18, #15233, .T. ) ;
#11007 = ORIENTED_EDGE ( 'NONE', *, *, #1344, .T. ) ;
#11008 = CARTESIAN_POINT ( 'NONE',  ( 31.44597781366222122, 27.99124249474150972, 70.25000000000000000 ) ) ;
#11009 = DIRECTION ( 'NONE',  ( -1.000000000000000000, 0.000000000000000000, 0.000000000000000000 ) ) ;
#11010 = CARTESIAN_POINT ( 'NONE',  ( -25.37540678000427263, -63.74634676501045050, 13.19999999999999929 ) ) ;
#11011 = VERTEX_POINT ( 'NONE', #16272 ) ;
#11012 = ORIENTED_EDGE ( 'NONE', *, *, #18082, .F. ) ;
#11013 = ORIENTED_EDGE ( 'NONE', *, *, #20692, .F. ) ;
#11014 = DIRECTION ( 'NONE',  ( 0.000000000000000000, 1.000000000000000000, 0.000000000000000000 ) ) ;
#11015 = AXIS2_PLACEMENT_3D ( 'NONE', #19206, #5795, #17525 ) ;
#11016 = CARTESIAN_POINT ( 'NONE',  ( 1.724728116533979838, 42.36054587065083155, 53.66679706732590915 ) ) ;
#11017 = ORIENTED_EDGE ( 'NONE', *, *, #14919, .F. ) ;
#11018 = DIRECTION ( 'NONE',  ( -1.000000000000000000, 0.000000000000000000, 0.000000000000000000 ) ) ;
#11019 = ADVANCED_FACE ( 'NONE', ( #13029 ), #1176, .T. ) ;
#11020 = EDGE_CURVE ( 'NONE', #877, #17577, #19775, .T. ) ;
#11021 = ORIENTED_EDGE ( 'NONE', *, *, #15854, .T. ) ;
#11022 = DIRECTION ( 'NONE',  ( 0.000000000000000000, 0.000000000000000000, -1.000000000000000000 ) ) ;
#11023 = VECTOR ( 'NONE', #21255, 1000.000000000000000 ) ;
#11024 = DIRECTION ( 'NONE',  ( 0.000000000000000000, 0.000000000000000000, 1.000000000000000000 ) ) ;
#11025 = EDGE_CURVE ( 'NONE', #17779, #8815, #18449, .T. ) ;
#11026 = LINE ( 'NONE', #13934, #12413 ) ;
#11027 = DIRECTION ( 'NONE',  ( 0.000000000000000000, 0.000000000000000000, 1.000000000000000000 ) ) ;
#11028 = AXIS2_PLACEMENT_3D ( 'NONE', #756, #2900, #6156 ) ;
#11029 = CARTESIAN_POINT ( 'NONE',  ( 14.96174975910705918, -32.10873716947361345, 13.05380965755522737 ) ) ;
#11030 = DIRECTION ( 'NONE',  ( 1.000000000000000000, 0.000000000000000000, 0.000000000000000000 ) ) ;
#11031 = VERTEX_POINT ( 'NONE', #8023 ) ;
#11032 = DIRECTION ( 'NONE',  ( 0.000000000000000000, 0.000000000000000000, 1.000000000000000000 ) ) ;
#11033 = AXIS2_PLACEMENT_3D ( 'NONE', #12489, #10501, #20806 ) ;
#11034 = DIRECTION ( 'NONE',  ( 0.000000000000000000, 0.000000000000000000, 1.000000000000000000 ) ) ;
#11035 = DIRECTION ( 'NONE',  ( 1.000000000000000000, 0.000000000000000000, 0.000000000000000000 ) ) ;
#11036 = CARTESIAN_POINT ( 'NONE',  ( -23.05999184077137443, -2.354728237135332414, 13.30000967910993737 ) ) ;
#11037 = ORIENTED_EDGE ( 'NONE', *, *, #114, .T. ) ;
#11038 =( NAMED_UNIT ( * ) PLANE_ANGLE_UNIT ( ) SI_UNIT ( $, .RADIAN. ) );
#11039 = EDGE_CURVE ( 'NONE', #16873, #3099, #12736, .T. ) ;
#11040 = EDGE_LOOP ( 'NONE', ( #4732, #4961, #4667, #12498 ) ) ;
#11041 = DIRECTION ( 'NONE',  ( -1.000000000000000000, -0.000000000000000000, -0.000000000000000000 ) ) ;
#11042 = DIRECTION ( 'NONE',  ( 0.000000000000000000, 0.000000000000000000, 1.000000000000000000 ) ) ;
#11043 = ORIENTED_EDGE ( 'NONE', *, *, #9429, .F. ) ;
#11044 = ORIENTED_EDGE ( 'NONE', *, *, #11541, .F. ) ;
#11045 = CARTESIAN_POINT ( 'NONE',  ( -26.37540678000427619, -10.94079601157914716, 13.50000000000000000 ) ) ;
#11046 = EDGE_CURVE ( 'NONE', #12088, #9996, #14826, .T. ) ;
#11047 = DIRECTION ( 'NONE',  ( 1.000000000000000000, 0.000000000000000000, -0.000000000000000000 ) ) ;
#11048 = CIRCLE ( 'NONE', #8895, 0.2500000000000002220 ) ;
#11049 = VERTEX_POINT ( 'NONE', #17970 ) ;
#11050 = AXIS2_PLACEMENT_3D ( 'NONE', #14636, #17882, #4460 ) ;
#11051 = ORIENTED_EDGE ( 'NONE', *, *, #4083, .F. ) ;
#11052 = ADVANCED_FACE ( 'NONE', ( #14485 ), #12707, .F. ) ;
#11053 = EDGE_LOOP ( 'NONE', ( #6435, #2860, #18953, #20206 ) ) ;
#11054 = CARTESIAN_POINT ( 'NONE',  ( -25.37540678000427263, -63.74634676501045050, 7.500000000000000000 ) ) ;
#11055 = LINE ( 'NONE', #1191, #10377 ) ;
#11056 = DIRECTION ( 'NONE',  ( 0.000000000000000000, 0.000000000000000000, 1.000000000000000000 ) ) ;
#11057 = CARTESIAN_POINT ( 'NONE',  ( -17.93704824106378837, 38.74634676501045760, 13.87500000000000000 ) ) ;
#11058 = CIRCLE ( 'NONE', #20024, 0.5000000000000004441 ) ;
#11059 = VECTOR ( 'NONE', #13205, 1000.000000000000000 ) ;
#11060 = CARTESIAN_POINT ( 'NONE',  ( -30.37540678000427619, 63.74634676501045050, 7.500000000000000000 ) ) ;
#11061 = ORIENTED_EDGE ( 'NONE', *, *, #14013, .T. ) ;
#11062 = CARTESIAN_POINT ( 'NONE',  ( 29.13662752439705272, 0.000000000000000000, 7.500000000000000000 ) ) ;
#11063 = LINE ( 'NONE', #18102, #19997 ) ;
#11064 = DIRECTION ( 'NONE',  ( 1.000000000000000000, 0.000000000000000000, 0.000000000000000000 ) ) ;
#11065 = FACE_OUTER_BOUND ( 'NONE', #1260, .T. ) ;
#11066 = EDGE_CURVE ( 'NONE', #5502, #12260, #6685, .T. ) ;
#11067 = CARTESIAN_POINT ( 'NONE',  ( 33.49999999999998579, -84.70000000000001705, 80.00000000000000000 ) ) ;
#11068 = ORIENTED_EDGE ( 'NONE', *, *, #15229, .T. ) ;
#11069 = EDGE_CURVE ( 'NONE', #15395, #10953, #4159, .T. ) ;
#11070 = ORIENTED_EDGE ( 'NONE', *, *, #18415, .F. ) ;
#11071 = VERTEX_POINT ( 'NONE', #14386 ) ;
#11072 = DIRECTION ( 'NONE',  ( 0.000000000000000000, 0.000000000000000000, -1.000000000000000000 ) ) ;
#11073 = AXIS2_PLACEMENT_3D ( 'NONE', #3760, #10584, #9240 ) ;
#11074 = CIRCLE ( 'NONE', #19661, 0.1000000000000028644 ) ;
#11075 = ORIENTED_EDGE ( 'NONE', *, *, #10757, .T. ) ;
#11076 = VECTOR ( 'NONE', #7889, 1000.000000000000000 ) ;
#11077 = ORIENTED_EDGE ( 'NONE', *, *, #9152, .T. ) ;
#11078 = ORIENTED_EDGE ( 'NONE', *, *, #12419, .T. ) ;
#11079 = CARTESIAN_POINT ( 'NONE',  ( -33.80000000000001847, -84.70000000000001705, 78.20000000000000284 ) ) ;
#11080 = ORIENTED_EDGE ( 'NONE', *, *, #9215, .T. ) ;
#11081 = DIRECTION ( 'NONE',  ( 0.000000000000000000, 1.000000000000000000, 0.000000000000000000 ) ) ;
#11082 = DIRECTION ( 'NONE',  ( 0.000000000000000000, 0.000000000000000000, -1.000000000000000000 ) ) ;
#11083 = CARTESIAN_POINT ( 'NONE',  ( -29.50000000000002132, 2.473451120191013430, 1.500000000000001332 ) ) ;
#11084 = DIRECTION ( 'NONE',  ( 0.000000000000000000, 0.000000000000000000, -1.000000000000000000 ) ) ;
#11085 = CIRCLE ( 'NONE', #8607, 0.2999999999999999334 ) ;
#11086 = AXIS2_PLACEMENT_3D ( 'NONE', #7196, #12423, #558 ) ;
#11087 = CARTESIAN_POINT ( 'NONE',  ( -1.724728116533986721, 42.36054587065083155, 39.75876104995654003 ) ) ;
#11088 = CARTESIAN_POINT ( 'NONE',  ( -25.37540678000427263, -63.74634676501045050, 7.500000000000000000 ) ) ;
#11089 = DIRECTION ( 'NONE',  ( 0.000000000000000000, 0.000000000000000000, -1.000000000000000000 ) ) ;
#11090 = EDGE_CURVE ( 'NONE', #8454, #11094, #19171, .T. ) ;
#11091 = DIRECTION ( 'NONE',  ( 0.000000000000000000, 0.000000000000000000, 1.000000000000000000 ) ) ;
#11092 = DIRECTION ( 'NONE',  ( 0.000000000000000000, 1.000000000000000000, 0.000000000000000000 ) ) ;
#11093 = ORIENTED_EDGE ( 'NONE', *, *, #9177, .T. ) ;
#11094 = VERTEX_POINT ( 'NONE', #2539 ) ;
#11095 = DIRECTION ( 'NONE',  ( 1.000000000000000000, 0.000000000000000000, -2.388292521039847891E-16 ) ) ;
#11096 = FILL_AREA_STYLE ('',( #21294 ) ) ;
#11097 = ORIENTED_EDGE ( 'NONE', *, *, #21217, .F. ) ;
#11098 = ORIENTED_EDGE ( 'NONE', *, *, #8, .T. ) ;
#11099 = PLANE ( 'NONE',  #19922 ) ;
#11100 = DIRECTION ( 'NONE',  ( -1.000000000000000000, 0.000000000000000000, 1.442933311647907116E-16 ) ) ;
#11101 = ORIENTED_EDGE ( 'NONE', *, *, #8726, .T. ) ;
#11102 = CIRCLE ( 'NONE', #2234, 0.2999999999999999334 ) ;
#11103 = CARTESIAN_POINT ( 'NONE',  ( 29.37540678000427619, 6.000000000000000000, 7.500000000000000000 ) ) ;
#11104 = AXIS2_PLACEMENT_3D ( 'NONE', #14851, #12015, #18864 ) ;
#11105 = DIRECTION ( 'NONE',  ( 1.000000000000000000, 0.000000000000000000, 0.000000000000000000 ) ) ;
#11106 = CARTESIAN_POINT ( 'NONE',  ( -1.824728116533986810, 42.36054587065083155, 45.71679706732590631 ) ) ;
#11107 = ADVANCED_FACE ( 'NONE', ( #8584 ), #19904, .F. ) ;
#11108 = ORIENTED_EDGE ( 'NONE', *, *, #21024, .F. ) ;
#11109 = CARTESIAN_POINT ( 'NONE',  ( 1.724728116533979616, 43.26054587065083012, 31.75876104995653648 ) ) ;
#11110 = CIRCLE ( 'NONE', #8277, 2.000000000000001776 ) ;
#11111 = DIRECTION ( 'NONE',  ( -1.000000000000000000, 0.000000000000000000, 2.107255972849994642E-16 ) ) ;
#11112 = EDGE_CURVE ( 'NONE', #18524, #12867, #5614, .T. ) ;
#11113 = DIRECTION ( 'NONE',  ( 1.000000000000000000, 0.000000000000000000, 0.000000000000000000 ) ) ;
#11114 = ORIENTED_EDGE ( 'NONE', *, *, #1895, .F. ) ;
#11115 = ORIENTED_EDGE ( 'NONE', *, *, #14595, .F. ) ;
#11116 = EDGE_LOOP ( 'NONE', ( #3564, #13468, #15646, #14496 ) ) ;
#11117 = CARTESIAN_POINT ( 'NONE',  ( 14.96174975910707161, 41.81054587065082728, 68.25000000000000000 ) ) ;
#11118 = DIRECTION ( 'NONE',  ( 0.07788375472025979573, 0.9969624470112574688, 0.000000000000000000 ) ) ;
#11119 = ORIENTED_EDGE ( 'NONE', *, *, #21260, .T. ) ;
#11120 = AXIS2_PLACEMENT_3D ( 'NONE', #1037, #21759, #1145 ) ;
#11121 = CIRCLE ( 'NONE', #13268, 0.05000000000000143219 ) ;
#11122 = CARTESIAN_POINT ( 'NONE',  ( 34.39999999999998437, -84.70000000000001705, 79.39999999999999147 ) ) ;
#11123 = AXIS2_PLACEMENT_3D ( 'NONE', #9551, #21760, #19623 ) ;
#11124 = VECTOR ( 'NONE', #17479, 999.9999999999998863 ) ;
#11125 = ORIENTED_EDGE ( 'NONE', *, *, #11516, .T. ) ;
#11126 = CARTESIAN_POINT ( 'NONE',  ( 30.79999999999999716, -84.70000000000001705, 1.200000000000004174 ) ) ;
#11127 = CARTESIAN_POINT ( 'NONE',  ( 32.50000000000002132, -71.00000000000001421, 3.500000000000000000 ) ) ;
#11128 = EDGE_CURVE ( 'NONE', #16858, #5434, #1400, .T. ) ;
#11129 = SPHERICAL_SURFACE ( 'NONE', #10646, 0.2500000000000000000 ) ;
#11130 = CARTESIAN_POINT ( 'NONE',  ( -30.37540678000427619, -63.74634676501045050, 7.200000000000000178 ) ) ;
#11131 = CARTESIAN_POINT ( 'NONE',  ( -1.724728116533986721, 43.31054587065082728, 39.80876104995653719 ) ) ;
#11132 = DIRECTION ( 'NONE',  ( 0.000000000000000000, 0.000000000000000000, 1.000000000000000000 ) ) ;
#11133 = ORIENTED_EDGE ( 'NONE', *, *, #280, .F. ) ;
#11134 = CARTESIAN_POINT ( 'NONE',  ( -21.92816239687475743, 42.46645089659918426, 68.50000000000000000 ) ) ;
#11135 = DIRECTION ( 'NONE',  ( -1.000000000000000000, -0.000000000000000000, -0.000000000000000000 ) ) ;
#11136 = CARTESIAN_POINT ( 'NONE',  ( -15.21174975910705207, 41.81054587065082728, 68.50000000000000000 ) ) ;
#11137 = DIRECTION ( 'NONE',  ( 0.000000000000000000, -0.000000000000000000, -1.000000000000000000 ) ) ;
#11138 = ORIENTED_EDGE ( 'NONE', *, *, #2961, .T. ) ;
#11139 = CIRCLE ( 'NONE', #6523, 2.000000000000001776 ) ;
#11140 = EDGE_CURVE ( 'NONE', #17289, #1639, #577, .T. ) ;
#11141 = AXIS2_PLACEMENT_3D ( 'NONE', #13544, #5052, #17126 ) ;
#11142 = ADVANCED_FACE ( 'NONE', ( #11479 ), #2982, .T. ) ;
#11143 = ORIENTED_EDGE ( 'NONE', *, *, #6782, .F. ) ;
#11144 = DIRECTION ( 'NONE',  ( 0.000000000000000000, 0.000000000000000000, -1.000000000000000000 ) ) ;
#11145 = EDGE_CURVE ( 'NONE', #20541, #8585, #18091, .T. ) ;
#11146 = CARTESIAN_POINT ( 'NONE',  ( -23.02398829872513630, -2.501746539338826292, 13.57884938331724101 ) ) ;
#11147 = ORIENTED_EDGE ( 'NONE', *, *, #15366, .F. ) ;
#11148 = ORIENTED_EDGE ( 'NONE', *, *, #9520, .F. ) ;
#11149 = FACE_OUTER_BOUND ( 'NONE', #13803, .T. ) ;
#11151 = EDGE_CURVE ( 'NONE', #1798, #12977, #8817, .T. ) ;
#11150 = DIRECTION ( 'NONE',  ( 0.000000000000000000, -0.000000000000000000, -1.000000000000000000 ) ) ;
#11152 = DIRECTION ( 'NONE',  ( 1.000000000000000000, 0.000000000000000000, 0.000000000000000000 ) ) ;
#11153 = VERTEX_POINT ( 'NONE', #21681 ) ;
#11154 = ORIENTED_EDGE ( 'NONE', *, *, #11285, .T. ) ;
#11155 = DIRECTION ( 'NONE',  ( 0.000000000000000000, 1.000000000000000000, 0.000000000000000000 ) ) ;
#11156 = VECTOR ( 'NONE', #7509, 1000.000000000000000 ) ;
#11157 = EDGE_CURVE ( 'NONE', #19467, #1047, #9920, .T. ) ;
#11158 = DIRECTION ( 'NONE',  ( -0.000000000000000000, 1.000000000000000000, 0.000000000000000000 ) ) ;
#11159 = CARTESIAN_POINT ( 'NONE',  ( -23.02398829872514341, -2.157133568461118589, 13.20000000000008100 ) ) ;
#11160 = CIRCLE ( 'NONE', #20778, 0.2500000000000002220 ) ;
#11161 = DIRECTION ( 'NONE',  ( -6.123233995736764803E-17, 0.000000000000000000, 1.000000000000000000 ) ) ;
#11162 = DIRECTION ( 'NONE',  ( 0.000000000000000000, 1.000000000000000000, -0.000000000000000000 ) ) ;
#11163 = CARTESIAN_POINT ( 'NONE',  ( -10.13407133124522730, 41.92645089659917801, 69.94509975324525897 ) ) ;
#11164 = CARTESIAN_POINT ( 'NONE',  ( -29.20000000000002061, -68.70000000000001705, 0.000000000000000000 ) ) ;
#11165 = VERTEX_POINT ( 'NONE', #6474 ) ;
#11166 = FACE_OUTER_BOUND ( 'NONE', #12183, .T. ) ;
#11167 = CIRCLE ( 'NONE', #3324, 0.2500000000000002220 ) ;
#11168 = DIRECTION ( 'NONE',  ( -0.9729678061520314891, -0.2309407893632107189, 0.000000000000000000 ) ) ;
#11169 = EDGE_CURVE ( 'NONE', #9425, #19429, #8246, .T. ) ;
#11170 = DIRECTION ( 'NONE',  ( -1.000000000000000000, 0.000000000000000000, 0.000000000000000000 ) ) ;
#11172 = EDGE_CURVE ( 'NONE', #13253, #2258, #13786, .T. ) ;
#11171 = DIRECTION ( 'NONE',  ( 0.000000000000000000, 0.000000000000000000, -1.000000000000000000 ) ) ;
#11173 = CARTESIAN_POINT ( 'NONE',  ( -1.774728116533986766, 43.26054587065083012, 33.66679706732590915 ) ) ;
#11174 = ORIENTED_EDGE ( 'NONE', *, *, #14548, .F. ) ;
#11175 = ORIENTED_EDGE ( 'NONE', *, *, #16616, .T. ) ;
#11176 = CARTESIAN_POINT ( 'NONE',  ( 29.69597781366221767, 27.99124249474150972, 68.75000000000000000 ) ) ;
#11177 = ORIENTED_EDGE ( 'NONE', *, *, #11970, .F. ) ;
#11178 = ORIENTED_EDGE ( 'NONE', *, *, #2869, .F. ) ;
#11179 = FILL_AREA_STYLE_COLOUR ( '', #11615 ) ;
#11180 = DIRECTION ( 'NONE',  ( -1.000000000000000000, 0.000000000000000000, 0.000000000000000000 ) ) ;
#11181 = ORIENTED_EDGE ( 'NONE', *, *, #11128, .F. ) ;
#11182 = LINE ( 'NONE', #17261, #364 ) ;
#11183 = VERTEX_POINT ( 'NONE', #13371 ) ;
#11184 = DIRECTION ( 'NONE',  ( 1.000000000000000000, 0.000000000000000000, 0.000000000000000000 ) ) ;
#11185 = ADVANCED_FACE ( 'NONE', ( #11576 ), #2006, .T. ) ;
#11186 = CARTESIAN_POINT ( 'NONE',  ( 29.50000000000002132, 0.000000000000000000, 1.500000000000000000 ) ) ;
#11187 = FACE_OUTER_BOUND ( 'NONE', #12024, .T. ) ;
#11188 = EDGE_CURVE ( 'NONE', #16682, #381, #18405, .T. ) ;
#11189 = DIRECTION ( 'NONE',  ( 0.000000000000000000, 0.000000000000000000, 1.000000000000000000 ) ) ;
#11190 = DIRECTION ( 'NONE',  ( -0.000000000000000000, -0.000000000000000000, -1.000000000000000000 ) ) ;
#11191 = DIRECTION ( 'NONE',  ( 2.107255972849994642E-16, -0.000000000000000000, 1.000000000000000000 ) ) ;
#11192 = DIRECTION ( 'NONE',  ( 0.000000000000000000, 1.000000000000000000, 0.000000000000000000 ) ) ;
#11193 = EDGE_CURVE ( 'NONE', #5317, #11913, #6356, .T. ) ;
#11194 = ORIENTED_EDGE ( 'NONE', *, *, #8561, .T. ) ;
#11195 = CYLINDRICAL_SURFACE ( 'NONE', #4529, 3.500000000000003109 ) ;
#11196 = PRESENTATION_LAYER_ASSIGNMENT (  '', '', ( #17264 ) ) ;
#11197 = DIRECTION ( 'NONE',  ( 3.052134192567367925E-16, 1.000000000000000000, -0.000000000000000000 ) ) ;
#11198 = ORIENTED_EDGE ( 'NONE', *, *, #11427, .T. ) ;
#11199 = ORIENTED_EDGE ( 'NONE', *, *, #7042, .T. ) ;
#11200 = DIRECTION ( 'NONE',  ( -2.388292521039847891E-16, 0.000000000000000000, -1.000000000000000000 ) ) ;
#11201 = ORIENTED_EDGE ( 'NONE', *, *, #487, .T. ) ;
#11202 = ORIENTED_EDGE ( 'NONE', *, *, #13925, .T. ) ;
#11203 = CIRCLE ( 'NONE', #2278, 0.5000000000000004441 ) ;
#11204 = ORIENTED_EDGE ( 'NONE', *, *, #2729, .T. ) ;
#11205 = FACE_OUTER_BOUND ( 'NONE', #19951, .T. ) ;
#11206 = AXIS2_PLACEMENT_3D ( 'NONE', #8395, #18576, #17001 ) ;
#11207 = PRODUCT_DEFINITION_FORMATION_WITH_SPECIFIED_SOURCE ( 'ANY', '', #15181, .NOT_KNOWN. ) ;
#11208 = EDGE_CURVE ( 'NONE', #6525, #833, #8350, .T. ) ;
#11209 = DIRECTION ( 'NONE',  ( -1.000000000000000000, -0.000000000000000000, -0.000000000000000000 ) ) ;
#11210 = TOROIDAL_SURFACE ( 'NONE', #3724, 2.076718556943726313, 0.2500000000000000000 ) ;
#11211 = ORIENTED_EDGE ( 'NONE', *, *, #6779, .F. ) ;
#11212 = DIRECTION ( 'NONE',  ( -0.000000000000000000, -0.000000000000000000, -1.000000000000000000 ) ) ;
#11213 = CARTESIAN_POINT ( 'NONE',  ( -3.127054932750481964, -32.61873716947361856, 68.00000000000000000 ) ) ;
#11214 = CARTESIAN_POINT ( 'NONE',  ( -28.86382559268571057, 6.505889654322387194, 13.29319881794719294 ) ) ;
#11215 = FACE_OUTER_BOUND ( 'NONE', #357, .T. ) ;
#11216 = CARTESIAN_POINT ( 'NONE',  ( -23.26716210542296182, 3.307210766252304701, 13.50000000000000355 ) ) ;
#11217 = ORIENTED_EDGE ( 'NONE', *, *, #15591, .F. ) ;
#11218 = CARTESIAN_POINT ( 'NONE',  ( 1.774728116533979660, 43.26054587065083012, 35.80876104995653009 ) ) ;
#11219 = DIRECTION ( 'NONE',  ( 1.734723475976806848E-16, -0.000000000000000000, -1.000000000000000000 ) ) ;
#11220 = ORIENTED_EDGE ( 'NONE', *, *, #34, .T. ) ;
#11221 = ORIENTED_EDGE ( 'NONE', *, *, #7746, .T. ) ;
#11222 = ORIENTED_EDGE ( 'NONE', *, *, #3375, .T. ) ;
#11223 = CARTESIAN_POINT ( 'NONE',  ( 14.96174975910705385, 51.80685496129630963, 13.81241846611418644 ) ) ;
#11224 = DIRECTION ( 'NONE',  ( 0.000000000000000000, 0.000000000000000000, 1.000000000000000000 ) ) ;
#11225 = ORIENTED_EDGE ( 'NONE', *, *, #2779, .T. ) ;
#11226 = ADVANCED_FACE ( 'NONE', ( #4997 ), #15058, .F. ) ;
#11227 = CARTESIAN_POINT ( 'NONE',  ( -32.23382792203229741, 83.71979900898287497, 68.25000000000000000 ) ) ;
#11228 = VERTEX_POINT ( 'NONE', #3421 ) ;
#11229 = CARTESIAN_POINT ( 'NONE',  ( 14.96174975910705918, -41.81054587065082728, 13.62426406871192874 ) ) ;
#11230 = DIRECTION ( 'NONE',  ( 1.000000000000000000, -0.000000000000000000, 0.000000000000000000 ) ) ;
#11231 = EDGE_CURVE ( 'NONE', #5864, #6786, #1747, .T. ) ;
#11232 = LINE ( 'NONE', #21663, #6385 ) ;
#11233 = DIRECTION ( 'NONE',  ( 0.000000000000000000, 0.000000000000000000, 1.000000000000000000 ) ) ;
#11234 = DIRECTION ( 'NONE',  ( 0.000000000000000000, 0.000000000000000000, 1.000000000000000000 ) ) ;
#11235 = CARTESIAN_POINT ( 'NONE',  ( -30.79999999999999361, -84.70000000000001705, 1.200000000000000400 ) ) ;
#11236 = VERTEX_POINT ( 'NONE', #13156 ) ;
#11237 = DIRECTION ( 'NONE',  ( 1.000000000000000000, -0.000000000000000000, -0.000000000000000000 ) ) ;
#11238 = CYLINDRICAL_SURFACE ( 'NONE', #13186, 0.05000000000000143219 ) ;
#11239 = DIRECTION ( 'NONE',  ( 0.000000000000000000, 0.000000000000000000, 1.000000000000000000 ) ) ;
#11240 = DIRECTION ( 'NONE',  ( 0.000000000000000000, 0.000000000000000000, 1.000000000000000000 ) ) ;
#11241 = ORIENTED_EDGE ( 'NONE', *, *, #5033, .F. ) ;
#11242 = AXIS2_PLACEMENT_3D ( 'NONE', #19543, #2537, #20005 ) ;
#11243 = VECTOR ( 'NONE', #7535, 1000.000000000000000 ) ;
#11244 = CARTESIAN_POINT ( 'NONE',  ( -8.134906293162361024, 41.92645089659918511, 68.06527860057354928 ) ) ;
#11245 = ORIENTED_EDGE ( 'NONE', *, *, #12935, .T. ) ;
#11246 = DIRECTION ( 'NONE',  ( -1.000000000000000000, 0.000000000000000000, 2.107255972849994642E-16 ) ) ;
#11247 = DIRECTION ( 'NONE',  ( -1.000000000000000000, 0.000000000000000000, 0.000000000000000000 ) ) ;
#11248 = ORIENTED_EDGE ( 'NONE', *, *, #2951, .T. ) ;
#11249 = ORIENTED_EDGE ( 'NONE', *, *, #6121, .F. ) ;
#11250 = CARTESIAN_POINT ( 'NONE',  ( -15.21174975910704852, 52.39333383871510108, 13.50000000000000000 ) ) ;
#11251 = DIRECTION ( 'NONE',  ( 0.000000000000000000, 0.000000000000000000, 1.000000000000000000 ) ) ;
#11252 = EDGE_CURVE ( 'NONE', #3127, #12578, #21697, .T. ) ;
#11253 = DIRECTION ( 'NONE',  ( 0.000000000000000000, 1.000000000000000000, 0.000000000000000000 ) ) ;
#11254 = EDGE_LOOP ( 'NONE', ( #15957, #14756, #2151, #17309, #4258, #9456 ) ) ;
#11255 = ORIENTED_EDGE ( 'NONE', *, *, #12512, .F. ) ;
#11256 = DIRECTION ( 'NONE',  ( 0.000000000000000000, 1.000000000000000000, 0.000000000000000000 ) ) ;
#11257 = AXIS2_PLACEMENT_3D ( 'NONE', #16840, #13263, #20207 ) ;
#11258 = EDGE_CURVE ( 'NONE', #11905, #3329, #3816, .T. ) ;
#11259 = CARTESIAN_POINT ( 'NONE',  ( -15.95292532278785913, -52.39333383871510108, 13.79999999999999716 ) ) ;
#11260 = DIRECTION ( 'NONE',  ( 0.000000000000000000, 0.000000000000000000, -1.000000000000000000 ) ) ;
#11261 = ADVANCED_FACE ( 'NONE', ( #12017 ), #4172, .T. ) ;
#11262 = PLANE ( 'NONE',  #7041 ) ;
#11263 = CARTESIAN_POINT ( 'NONE',  ( 25.37540678000427263, 67.24634676501045760, 13.50000000000000000 ) ) ;
#11264 = DIRECTION ( 'NONE',  ( -1.000000000000000000, -3.491481338843133355E-15, 1.224646799147353207E-16 ) ) ;
#11265 = VERTEX_POINT ( 'NONE', #9012 ) ;
#11266 = CARTESIAN_POINT ( 'NONE',  ( -9.178906393579156386, 42.46645089659917716, 69.50000000000000000 ) ) ;
#11267 = DIRECTION ( 'NONE',  ( 1.000000000000000000, 0.000000000000000000, 0.000000000000000000 ) ) ;
#11268 = LINE ( 'NONE', #16430, #12103 ) ;
#11269 = EDGE_LOOP ( 'NONE', ( #11119, #7264, #12701, #13495, #14361 ) ) ;
#11270 = DIRECTION ( 'NONE',  ( 0.000000000000000000, 0.000000000000000000, 1.000000000000000000 ) ) ;
#11271 = TOROIDAL_SURFACE ( 'NONE', #16991, 0.05000000000000000278, 0.05000000000000000278 ) ;
#11272 = DIRECTION ( 'NONE',  ( 0.000000000000000000, 0.000000000000000000, 1.000000000000000000 ) ) ;
#11273 = DIRECTION ( 'NONE',  ( 0.000000000000000000, 0.000000000000000000, 1.000000000000000000 ) ) ;
#11274 = VERTEX_POINT ( 'NONE', #12455 ) ;
#11275 = CIRCLE ( 'NONE', #1631, 0.5000000000000004441 ) ;
#11276 = CIRCLE ( 'NONE', #9496, 1.000000000000000000 ) ;
#11277 = CIRCLE ( 'NONE', #1633, 0.05000000000000143219 ) ;
#11278 = DIRECTION ( 'NONE',  ( 1.000000000000000000, 0.000000000000000000, 0.000000000000000000 ) ) ;
#11279 = EDGE_CURVE ( 'NONE', #13182, #15775, #3750, .T. ) ;
#11280 = CARTESIAN_POINT ( 'NONE',  ( -33.80000000000000426, 84.70000000000001705, 1.800000000000000266 ) ) ;
#11281 = VERTEX_POINT ( 'NONE', #2281 ) ;
#11282 = DIRECTION ( 'NONE',  ( 1.000000000000000000, 0.000000000000000000, 0.000000000000000000 ) ) ;
#11283 = AXIS2_PLACEMENT_3D ( 'NONE', #17629, #10713, #2198 ) ;
#11284 = AXIS2_PLACEMENT_3D ( 'NONE', #15311, #21822, #5253 ) ;
#11285 = EDGE_CURVE ( 'NONE', #19432, #19665, #2023, .T. ) ;
#11286 = CARTESIAN_POINT ( 'NONE',  ( 27.37540678000427619, 5.683640910026986681, 13.50000000000000000 ) ) ;
#11287 = DIRECTION ( 'NONE',  ( -0.000000000000000000, 0.000000000000000000, 1.000000000000000000 ) ) ;
#11288 = ADVANCED_FACE ( 'NONE', ( #20983 ), #11669, .T. ) ;
#11289 = AXIS2_PLACEMENT_3D ( 'NONE', #13908, #7435, #5537 ) ;
#11290 = EDGE_LOOP ( 'NONE', ( #3814, #6465, #20, #10166, #2964, #9088, #12897, #11658 ) ) ;
#11291 = EDGE_CURVE ( 'NONE', #6266, #6508, #7054, .T. ) ;
#11292 = CARTESIAN_POINT ( 'NONE',  ( -20.10144383993102934, 42.46645089659918426, 68.25000000000000000 ) ) ;
#11293 = LINE ( 'NONE', #2809, #20605 ) ;
#11294 = CARTESIAN_POINT ( 'NONE',  ( 25.37540678000427263, -63.74634676501045050, 7.500000000000000000 ) ) ;
#11295 = DIRECTION ( 'NONE',  ( -0.000000000000000000, 1.000000000000000000, -0.000000000000000000 ) ) ;
#11296 = CARTESIAN_POINT ( 'NONE',  ( -21.69312596654449621, 45.47506926072997402, 68.25000000000000000 ) ) ;
#11297 = DIRECTION ( 'NONE',  ( -0.000000000000000000, -1.000000000000000000, -0.000000000000000000 ) ) ;
#11298 = AXIS2_PLACEMENT_3D ( 'NONE', #16593, #20191, #16388 ) ;
#11299 = DIRECTION ( 'NONE',  ( -0.000000000000000000, -1.000000000000000000, -0.000000000000000000 ) ) ;
#11300 = VECTOR ( 'NONE', #11237, 1000.000000000000000 ) ;
#11301 = AXIS2_PLACEMENT_3D ( 'NONE', #12690, #6029, #740 ) ;
#11302 = CIRCLE ( 'NONE', #18811, 0.2999999999999999334 ) ;
#11303 = ORIENTED_EDGE ( 'NONE', *, *, #6768, .T. ) ;
#11304 = CARTESIAN_POINT ( 'NONE',  ( 8.641460742840918030, 32.93424481021354921, 68.50000000000000000 ) ) ;
#11305 = DIRECTION ( 'NONE',  ( 1.000000000000000000, 0.000000000000000000, 1.734723475976786140E-16 ) ) ;
#11306 = ORIENTED_EDGE ( 'NONE', *, *, #3173, .F. ) ;
#11307 = VECTOR ( 'NONE', #13426, 1000.000000000000000 ) ;
#11308 = ORIENTED_EDGE ( 'NONE', *, *, #9821, .T. ) ;
#11309 = DIRECTION ( 'NONE',  ( 0.000000000000000000, 0.000000000000000000, -1.000000000000000000 ) ) ;
#11310 = EDGE_CURVE ( 'NONE', #3678, #18476, #19191, .T. ) ;
#11311 = UNCERTAINTY_MEASURE_WITH_UNIT (LENGTH_MEASURE( 1.000000000000000082E-05 ), #450, 'distance_accuracy_value', 'NONE');
#11312 = ORIENTED_EDGE ( 'NONE', *, *, #5662, .F. ) ;
#11313 = VERTEX_POINT ( 'NONE', #2175 ) ;
#11314 = ORIENTED_EDGE ( 'NONE', *, *, #10993, .T. ) ;
#11315 = AXIS2_PLACEMENT_3D ( 'NONE', #3855, #14113, #2160 ) ;
#11316 = CIRCLE ( 'NONE', #14520, 0.05000000000000143219 ) ;
#11317 = AXIS2_PLACEMENT_3D ( 'NONE', #20266, #17005, #10092 ) ;
#11318 = VERTEX_POINT ( 'NONE', #8789 ) ;
#11319 = EDGE_CURVE ( 'NONE', #18476, #258, #5632, .T. ) ;
#11320 = VECTOR ( 'NONE', #16530, 1000.000000000000000 ) ;
#11321 = CARTESIAN_POINT ( 'NONE',  ( 15.07117748393522483, -52.06955913406978453, 13.87289863735440321 ) ) ;
#11322 = VECTOR ( 'NONE', #12791, 1000.000000000000000 ) ;
#11323 = DIRECTION ( 'NONE',  ( 0.000000000000000000, -0.000000000000000000, -1.000000000000000000 ) ) ;
#11324 = VECTOR ( 'NONE', #21354, 1000.000000000000000 ) ;
#11325 = ORIENTED_EDGE ( 'NONE', *, *, #8031, .F. ) ;
#11326 = DIRECTION ( 'NONE',  ( 1.000000000000000000, 0.000000000000000000, 0.000000000000000000 ) ) ;
#11327 = CARTESIAN_POINT ( 'NONE',  ( -9.178906393579158163, 42.46645089659918426, 68.06527860057354928 ) ) ;
#11328 = FACE_OUTER_BOUND ( 'NONE', #12341, .T. ) ;
#11329 = CARTESIAN_POINT ( 'NONE',  ( -23.21392692125925805, 3.086569931169079073, 13.48002932626963712 ) ) ;
#11330 = ORIENTED_EDGE ( 'NONE', *, *, #21503, .F. ) ;
#11331 = CARTESIAN_POINT ( 'NONE',  ( 15.21174975910705918, -52.39333383871510108, 13.50000000000000000 ) ) ;
#11332 = CYLINDRICAL_SURFACE ( 'NONE', #12698, 0.04999999999999991257 ) ;
#11333 = VECTOR ( 'NONE', #14624, 1000.000000000000000 ) ;
#11334 = EDGE_LOOP ( 'NONE', ( #2012, #19551, #8208, #4672 ) ) ;
#11335 = CIRCLE ( 'NONE', #6368, 3.200000000000001510 ) ;
#11336 = CIRCLE ( 'NONE', #617, 2.274596669241485181 ) ;
#11337 = EDGE_LOOP ( 'NONE', ( #14693, #993, #5247, #7587 ) ) ;
#11338 = ORIENTED_EDGE ( 'NONE', *, *, #8093, .T. ) ;
#11339 = FACE_OUTER_BOUND ( 'NONE', #11503, .T. ) ;
#11341 = EDGE_CURVE ( 'NONE', #4433, #8987, #19302, .T. ) ;
#11340 = FACE_OUTER_BOUND ( 'NONE', #3887, .T. ) ;
#11342 = ORIENTED_EDGE ( 'NONE', *, *, #1642, .F. ) ;
#11343 = VECTOR ( 'NONE', #20777, 1000.000000000000000 ) ;
#11344 = EDGE_CURVE ( 'NONE', #14491, #14946, #271, .T. ) ;
#11345 = CARTESIAN_POINT ( 'NONE',  ( -31.26086011588027347, 83.95073979834609190, 68.25000000000000000 ) ) ;
#11346 = AXIS2_PLACEMENT_3D ( 'NONE', #21982, #1827, #11887 ) ;
#11347 = AXIS2_PLACEMENT_3D ( 'NONE', #18019, #4488, #4727 ) ;
#11348 = ORIENTED_EDGE ( 'NONE', *, *, #14104, .F. ) ;
#11349 = DIRECTION ( 'NONE',  ( -1.000000000000000000, 0.000000000000000000, 0.000000000000000000 ) ) ;
#11350 = CARTESIAN_POINT ( 'NONE',  ( -9.141460742840918030, 32.61873716947361856, 68.50000000000000000 ) ) ;
#11351 = CARTESIAN_POINT ( 'NONE',  ( 3.127054932750481964, -32.11873716947361856, 68.00000000000000000 ) ) ;
#11352 = DIRECTION ( 'NONE',  ( 0.000000000000000000, -0.000000000000000000, -1.000000000000000000 ) ) ;
#11353 = VECTOR ( 'NONE', #21332, 1000.000000000000000 ) ;
#11354 = TOROIDAL_SURFACE ( 'NONE', #1710, 0.2500000000000000000, 0.2500000000000000000 ) ;
#11355 = CARTESIAN_POINT ( 'NONE',  ( 0.000000000000000000, 32.11873716947361856, 42.50000000000000711 ) ) ;
#11356 = CARTESIAN_POINT ( 'NONE',  ( -21.92816239687475743, 42.46645089659918426, 68.50000000000000000 ) ) ;
#11357 = ORIENTED_EDGE ( 'NONE', *, *, #18292, .T. ) ;
#11358 = LINE ( 'NONE', #2867, #11300 ) ;
#11359 = FACE_OUTER_BOUND ( 'NONE', #10936, .T. ) ;
#11360 = AXIS2_PLACEMENT_3D ( 'NONE', #11266, #8043, #4243 ) ;
#11361 = DIRECTION ( 'NONE',  ( 0.000000000000000000, 0.000000000000000000, -1.000000000000000000 ) ) ;
#11362 = ORIENTED_EDGE ( 'NONE', *, *, #7467, .T. ) ;
#11363 = EDGE_CURVE ( 'NONE', #20718, #20941, #18556, .T. ) ;
#11364 = DIRECTION ( 'NONE',  ( -0.000000000000000000, 0.000000000000000000, 1.000000000000000000 ) ) ;
#11365 = AXIS2_PLACEMENT_3D ( 'NONE', #19, #3157, #6633 ) ;
#11366 = DIRECTION ( 'NONE',  ( 0.000000000000000000, 0.000000000000000000, 1.000000000000000000 ) ) ;
#11367 = AXIS2_PLACEMENT_3D ( 'NONE', #9028, #5568, #11027 ) ;
#11368 = ORIENTED_EDGE ( 'NONE', *, *, #7989, .T. ) ;
#11369 = CARTESIAN_POINT ( 'NONE',  ( 1.724728116533979616, 43.26054587065083012, 41.76679706732590347 ) ) ;
#11370 = DIRECTION ( 'NONE',  ( 1.000000000000000000, 0.000000000000000000, 0.000000000000000000 ) ) ;
#11371 = ORIENTED_EDGE ( 'NONE', *, *, #21873, .F. ) ;
#11372 = ORIENTED_EDGE ( 'NONE', *, *, #20023, .F. ) ;
#11373 = ORIENTED_EDGE ( 'NONE', *, *, #19642, .F. ) ;
#11374 = CARTESIAN_POINT ( 'NONE',  ( -15.21174975910705207, 52.39333383871510108, 13.50000000000000000 ) ) ;
#11375 = CARTESIAN_POINT ( 'NONE',  ( 25.37540678000427263, -69.04634676501045476, 3.500000000000000000 ) ) ;
#11376 = EDGE_CURVE ( 'NONE', #8891, #11318, #14521, .T. ) ;
#11377 = FACE_OUTER_BOUND ( 'NONE', #18716, .T. ) ;
#11378 = AXIS2_PLACEMENT_3D ( 'NONE', #7597, #21245, #21688 ) ;
#11379 = ORIENTED_EDGE ( 'NONE', *, *, #9151, .T. ) ;
#11380 = VECTOR ( 'NONE', #10491, 1000.000000000000000 ) ;
#11381 = ORIENTED_EDGE ( 'NONE', *, *, #8, .F. ) ;
#11382 = DIRECTION ( 'NONE',  ( 0.000000000000000000, 1.000000000000000000, 0.000000000000000000 ) ) ;
#11383 = VECTOR ( 'NONE', #11455, 1000.000000000000000 ) ;
#11384 = CIRCLE ( 'NONE', #1743, 1.750000000000001554 ) ;
#11385 = LINE ( 'NONE', #9822, #13121 ) ;
#11386 = CARTESIAN_POINT ( 'NONE',  ( -23.02398829872513986, -2.334736181298132873, 13.36928379767489439 ) ) ;
#11387 = CARTESIAN_POINT ( 'NONE',  ( -25.37540678000427263, -63.74634676501045050, 7.500000000000000000 ) ) ;
#11388 = DIRECTION ( 'NONE',  ( -1.000000000000000000, -0.000000000000000000, -0.000000000000000000 ) ) ;
#11389 = LINE ( 'NONE', #8157, #21186 ) ;
#11390 = DIRECTION ( 'NONE',  ( 0.000000000000000000, -1.000000000000000000, 0.000000000000000000 ) ) ;
#11391 = ADVANCED_FACE ( 'NONE', ( #20547 ), #12233, .F. ) ;
#11392 = LINE ( 'NONE', #8044, #8832 ) ;
#11393 = VERTEX_POINT ( 'NONE', #19082 ) ;
#11394 = CIRCLE ( 'NONE', #19262, 3.017785046117004377 ) ;
#11395 = DIRECTION ( 'NONE',  ( 0.000000000000000000, 0.000000000000000000, -1.000000000000000000 ) ) ;
#11396 = DIRECTION ( 'NONE',  ( -0.000000000000000000, -1.000000000000000000, -0.000000000000000000 ) ) ;
#11397 = AXIS2_PLACEMENT_3D ( 'NONE', #7222, #12321, #10559 ) ;
#11398 = FACE_OUTER_BOUND ( 'NONE', #13841, .T. ) ;
#11399 = ORIENTED_EDGE ( 'NONE', *, *, #842, .F. ) ;
#11400 = ADVANCED_FACE ( 'NONE', ( #3543 ), #20642, .T. ) ;
#11401 = TOROIDAL_SURFACE ( 'NONE', #9269, 0.05000000000000000278, 0.05000000000000000278 ) ;
#11402 = EDGE_CURVE ( 'NONE', #3263, #6391, #19538, .T. ) ;
#11403 = DIRECTION ( 'NONE',  ( 0.000000000000000000, 1.000000000000000000, -0.000000000000000000 ) ) ;
#11404 = ORIENTED_EDGE ( 'NONE', *, *, #12206, .T. ) ;
#11405 = ADVANCED_FACE ( 'NONE', ( #12130 ), #14897, .T. ) ;
#11406 = VERTEX_POINT ( 'NONE', #3650 ) ;
#11407 = CYLINDRICAL_SURFACE ( 'NONE', #11732, 0.5000000000000000000 ) ;
#11408 = VERTEX_POINT ( 'NONE', #8077 ) ;
#11409 = CYLINDRICAL_SURFACE ( 'NONE', #17927, 0.2999999999999947153 ) ;
#11410 = CARTESIAN_POINT ( 'NONE',  ( -29.13662752439705272, 0.000000000000000000, 13.50000000000000000 ) ) ;
#11411 = CIRCLE ( 'NONE', #21426, 0.5000000000000004441 ) ;
#11412 = FACE_OUTER_BOUND ( 'NONE', #14109, .T. ) ;
#11413 = DIRECTION ( 'NONE',  ( 0.000000000000000000, 0.000000000000000000, 1.000000000000000000 ) ) ;
#11414 = EDGE_CURVE ( 'NONE', #13975, #6455, #6415, .T. ) ;
#11415 = CARTESIAN_POINT ( 'NONE',  ( -14.96174975910705207, 50.19799549595485644, 13.75000000000000000 ) ) ;
#11416 = DIRECTION ( 'NONE',  ( -0.000000000000000000, -0.000000000000000000, -1.000000000000000000 ) ) ;
#11417 = DIRECTION ( 'NONE',  ( 1.301042606982568087E-14, 0.000000000000000000, 1.000000000000000000 ) ) ;
#11418 = CYLINDRICAL_SURFACE ( 'NONE', #17240, 0.3000000000000016542 ) ;
#11419 = DIRECTION ( 'NONE',  ( -0.000000000000000000, -0.000000000000000000, -1.000000000000000000 ) ) ;
#11420 = CARTESIAN_POINT ( 'NONE',  ( -10.05825507651048412, 43.00645089659918341, 69.00503344894275415 ) ) ;
#11421 = ADVANCED_FACE ( 'NONE', ( #14883 ), #3106, .F. ) ;
#11422 = ORIENTED_EDGE ( 'NONE', *, *, #8536, .T. ) ;
#11423 = ORIENTED_EDGE ( 'NONE', *, *, #17372, .T. ) ;
#11424 = CARTESIAN_POINT ( 'NONE',  ( 1.824728116533979705, 43.26054587065083012, 49.66679706732590915 ) ) ;
#11425 = AXIS2_PLACEMENT_3D ( 'NONE', #16422, #7606, #9273 ) ;
#11426 = AXIS2_PLACEMENT_3D ( 'NONE', #11917, #1753, #12027 ) ;
#11427 = EDGE_CURVE ( 'NONE', #16763, #12996, #5276, .T. ) ;
#11428 = PRODUCT ( 'Main Body', 'Main Body', '', ( #7288 ) ) ;
#11429 = VERTEX_POINT ( 'NONE', #3033 ) ;
#11430 = ORIENTED_EDGE ( 'NONE', *, *, #19963, .T. ) ;
#11431 = CARTESIAN_POINT ( 'NONE',  ( 17.95292532278785913, 0.000000000000000000, 68.00000000000000000 ) ) ;
#11432 = EDGE_CURVE ( 'NONE', #17106, #9117, #953, .T. ) ;
#11433 = DIRECTION ( 'NONE',  ( 1.000000000000000000, 0.000000000000000000, 0.000000000000000000 ) ) ;
#11434 = ORIENTED_EDGE ( 'NONE', *, *, #7605, .F. ) ;
#11435 = ORIENTED_EDGE ( 'NONE', *, *, #21397, .T. ) ;
#11436 = VERTEX_POINT ( 'NONE', #17827 ) ;
#11437 =( REPRESENTATION_RELATIONSHIP ('NONE','NONE', #561, #10840 ) REPRESENTATION_RELATIONSHIP_WITH_TRANSFORMATION ( #5618 )SHAPE_REPRESENTATION_RELATIONSHIP( ) );
#11438 = AXIS2_PLACEMENT_3D ( 'NONE', #4760, #6900, #21888 ) ;
#11439 = ADVANCED_FACE ( 'NONE', ( #21104 ), #7452, .T. ) ;
#11440 = CARTESIAN_POINT ( 'NONE',  ( -14.75141514895150152, -52.14252005765846576, 13.50000000000000355 ) ) ;
#11441 = AXIS2_PLACEMENT_3D ( 'NONE', #153, #7002, #13792 ) ;
#11442 = DIRECTION ( 'NONE',  ( 0.000000000000000000, -1.000000000000000000, 0.000000000000000000 ) ) ;
#11443 = ORIENTED_EDGE ( 'NONE', *, *, #6815, .F. ) ;
#11444 = SURFACE_SIDE_STYLE ('',( #19967 ) ) ;
#11445 = EDGE_CURVE ( 'NONE', #5841, #15631, #3834, .T. ) ;
#11446 = DIRECTION ( 'NONE',  ( 1.734723475976806848E-16, -0.000000000000000000, -1.000000000000000000 ) ) ;
#11447 = CARTESIAN_POINT ( 'NONE',  ( 0.000000000000000000, 43.31054587065082728, 0.000000000000000000 ) ) ;
#11448 = CARTESIAN_POINT ( 'NONE',  ( -23.06007706085599906, 2.355179835980773628, 13.30024289742314636 ) ) ;
#11449 = EDGE_LOOP ( 'NONE', ( #10802, #10669, #18624, #13032 ) ) ;
#11450 = EDGE_LOOP ( 'NONE', ( #19744, #17550, #17829, #13160 ) ) ;
#11451 = ORIENTED_EDGE ( 'NONE', *, *, #18615, .T. ) ;
#11452 = CARTESIAN_POINT ( 'NONE',  ( -1.774728116533986766, 43.26054587065083012, 29.66679706732590560 ) ) ;
#11453 = ADVANCED_FACE ( 'NONE', ( #17714 ), #12785, .F. ) ;
#11454 = CIRCLE ( 'NONE', #18934, 0.2999999999999999334 ) ;
#11455 = DIRECTION ( 'NONE',  ( 0.000000000000000000, -1.000000000000000000, 0.000000000000000000 ) ) ;
#11456 = ORIENTED_EDGE ( 'NONE', *, *, #15164, .T. ) ;
#11457 = CIRCLE ( 'NONE', #19678, 0.05000000000000143219 ) ;
#11458 = DIRECTION ( 'NONE',  ( -1.000000000000000000, -0.000000000000000000, -0.000000000000000000 ) ) ;
#11459 = VERTEX_POINT ( 'NONE', #709 ) ;
#11460 = DIRECTION ( 'NONE',  ( 0.000000000000000000, 0.000000000000000000, -1.000000000000000000 ) ) ;
#11461 = CARTESIAN_POINT ( 'NONE',  ( -1.774728116533986766, 43.31054587065082728, 33.66679706732590915 ) ) ;
#11462 = LINE ( 'NONE', #18054, #18880 ) ;
#11463 = CYLINDRICAL_SURFACE ( 'NONE', #7374, 0.2999999999999999334 ) ;
#11464 = EDGE_LOOP ( 'NONE', ( #20085, #21407, #12355, #4946, #19699, #18529 ) ) ;
#11465 = DIRECTION ( 'NONE',  ( 0.000000000000000000, 0.000000000000000000, -1.000000000000000000 ) ) ;
#11466 = CARTESIAN_POINT ( 'NONE',  ( -8.299557710647832209, 41.92645089659918511, 69.00503344894275415 ) ) ;
#11467 = EDGE_CURVE ( 'NONE', #17196, #5035, #4078, .T. ) ;
#11468 = VECTOR ( 'NONE', #15290, 1000.000000000000000 ) ;
#11469 = EDGE_CURVE ( 'NONE', #17779, #19855, #20056, .T. ) ;
#11470 = DIRECTION ( 'NONE',  ( 1.000000000000000000, 0.000000000000000000, 0.000000000000000000 ) ) ;
#11471 = DIRECTION ( 'NONE',  ( 0.000000000000000000, 0.000000000000000000, 1.000000000000000000 ) ) ;
#11472 = ORIENTED_EDGE ( 'NONE', *, *, #3146, .F. ) ;
#11473 = EDGE_CURVE ( 'NONE', #11408, #17187, #4901, .T. ) ;
#11474 = LINE ( 'NONE', #19077, #6656 ) ;
#11475 = DIRECTION ( 'NONE',  ( 0.000000000000000000, -1.000000000000000000, 0.000000000000000000 ) ) ;
#11476 = DIRECTION ( 'NONE',  ( 1.000000000000000000, 0.000000000000000000, 0.000000000000000000 ) ) ;
#11477 = ORIENTED_EDGE ( 'NONE', *, *, #4017, .F. ) ;
#11478 = CARTESIAN_POINT ( 'NONE',  ( -29.69597781366221412, 26.24124249474150972, 70.25000000000000000 ) ) ;
#11479 = FACE_OUTER_BOUND ( 'NONE', #21105, .T. ) ;
#11480 = ORIENTED_EDGE ( 'NONE', *, *, #7668, .F. ) ;
#11481 = ORIENTED_EDGE ( 'NONE', *, *, #1138, .T. ) ;
#11482 = EDGE_LOOP ( 'NONE', ( #464, #10922, #14350, #10984 ) ) ;
#11483 = DIRECTION ( 'NONE',  ( 0.000000000000000000, 0.000000000000000000, 1.000000000000000000 ) ) ;
#11484 = CIRCLE ( 'NONE', #11123, 0.05000000000000143219 ) ;
#11485 = CARTESIAN_POINT ( 'NONE',  ( 3.127054932750481964, 32.93424481021354921, 68.00000000000000000 ) ) ;
#11486 = CIRCLE ( 'NONE', #3622, 5.193574995607838751 ) ;
#11487 = ORIENTED_EDGE ( 'NONE', *, *, #1298, .T. ) ;
#11488 = ORIENTED_EDGE ( 'NONE', *, *, #880, .T. ) ;
#11489 = CARTESIAN_POINT ( 'NONE',  ( -32.23382792203229741, 83.71979900898287497, 68.25000000000000000 ) ) ;
#11490 = CYLINDRICAL_SURFACE ( 'NONE', #18125, 0.5000000000000004441 ) ;
#11491 = CARTESIAN_POINT ( 'NONE',  ( -23.32398829872514057, 7.118794219358020148E-15, 13.50000000000000000 ) ) ;
#11492 = DIRECTION ( 'NONE',  ( 0.000000000000000000, 0.000000000000000000, 1.000000000000000000 ) ) ;
#11493 = AXIS2_PLACEMENT_3D ( 'NONE', #5358, #9128, #5569 ) ;
#11494 = CARTESIAN_POINT ( 'NONE',  ( 18.22752199202934520, 50.11873716947361856, 13.50000000000000000 ) ) ;
#11495 = CARTESIAN_POINT ( 'NONE',  ( 33.19999999999999574, 84.70000000000001705, 1.200000000000004174 ) ) ;
#11496 = LINE ( 'NONE', #18325, #4953 ) ;
#11497 = ADVANCED_FACE ( 'NONE', ( #8197 ), #4188, .T. ) ;
#11498 = AXIS2_PLACEMENT_3D ( 'NONE', #13888, #12634, #15678 ) ;
#11499 = CONICAL_SURFACE ( 'NONE', #8663, 4.575000000000001066, 0.8028514559173934861 ) ;
#11500 = AXIS2_PLACEMENT_3D ( 'NONE', #16371, #21432, #19973 ) ;
#11501 = LINE ( 'NONE', #9829, #20265 ) ;
#11502 = DIRECTION ( 'NONE',  ( -1.000000000000000000, 0.000000000000000000, 0.000000000000000000 ) ) ;
#11503 = EDGE_LOOP ( 'NONE', ( #3351, #4640, #2615, #1537 ) ) ;
#11504 = EDGE_CURVE ( 'NONE', #2381, #12853, #2396, .T. ) ;
#11505 = CYLINDRICAL_SURFACE ( 'NONE', #529, 2.000000000000001776 ) ;
#11506 = CARTESIAN_POINT ( 'NONE',  ( 14.37248138918699425, 42.46645089659917716, 69.50000000000000000 ) ) ;
#11507 = VERTEX_POINT ( 'NONE', #16138 ) ;
#11508 = CARTESIAN_POINT ( 'NONE',  ( -1.724728116533986721, 43.26054587065083012, 47.80876104995653719 ) ) ;
#11509 = DIRECTION ( 'NONE',  ( 1.000000000000000000, 0.000000000000000000, 0.000000000000000000 ) ) ;
#11510 = VERTEX_POINT ( 'NONE', #16670 ) ;
#11511 = VERTEX_POINT ( 'NONE', #7660 ) ;
#11512 = FACE_OUTER_BOUND ( 'NONE', #6448, .T. ) ;
#11513 = AXIS2_PLACEMENT_3D ( 'NONE', #6055, #17992, #2666 ) ;
#11514 = AXIS2_PLACEMENT_3D ( 'NONE', #4242, #9274, #14182 ) ;
#11515 = ORIENTED_EDGE ( 'NONE', *, *, #7601, .F. ) ;
#11516 = EDGE_CURVE ( 'NONE', #19066, #15364, #8133, .T. ) ;
#11517 = DIRECTION ( 'NONE',  ( 0.000000000000000000, 0.000000000000000000, 1.000000000000000000 ) ) ;
#11518 = LINE ( 'NONE', #1330, #2751 ) ;
#11519 = DIRECTION ( 'NONE',  ( 0.000000000000000000, -1.000000000000000000, 0.000000000000000000 ) ) ;
#11520 = CIRCLE ( 'NONE', #13308, 2.000000000000000000 ) ;
#11521 = EDGE_CURVE ( 'NONE', #14169, #20520, #18353, .T. ) ;
#11522 = DIRECTION ( 'NONE',  ( 1.000000000000000000, 0.000000000000000000, 0.000000000000000000 ) ) ;
#11523 = DIRECTION ( 'NONE',  ( 0.000000000000000000, 0.000000000000000000, -1.000000000000000000 ) ) ;
#11524 = FACE_OUTER_BOUND ( 'NONE', #12978, .T. ) ;
#11525 = CARTESIAN_POINT ( 'NONE',  ( 23.02398829872513986, 3.528912754968628551, 13.79999999999999893 ) ) ;
#11526 = CARTESIAN_POINT ( 'NONE',  ( -9.978973617317267397, 43.00645089659918341, 68.06527860057354928 ) ) ;
#11527 = CARTESIAN_POINT ( 'NONE',  ( -29.13662752439705272, 0.000000000000000000, 7.200000000000000178 ) ) ;
#11528 = ORIENTED_EDGE ( 'NONE', *, *, #9485, .F. ) ;
#11529 = DIRECTION ( 'NONE',  ( 1.000000000000000000, 0.000000000000000000, 0.000000000000000000 ) ) ;
#11530 = FACE_OUTER_BOUND ( 'NONE', #10426, .T. ) ;
#11531 = ORIENTED_EDGE ( 'NONE', *, *, #7720, .F. ) ;
#11532 = ORIENTED_EDGE ( 'NONE', *, *, #7716, .T. ) ;
#11533 = LINE ( 'NONE', #16906, #16356 ) ;
#11534 = SURFACE_STYLE_USAGE ( .BOTH. , #9764 ) ;
#11535 = ADVANCED_FACE ( 'NONE', ( #6527 ), #13319, .F. ) ;
#11536 = ORIENTED_EDGE ( 'NONE', *, *, #8347, .F. ) ;
#11537 = DIRECTION ( 'NONE',  ( 0.000000000000000000, -1.000000000000000000, 0.000000000000000000 ) ) ;
#11538 = ORIENTED_EDGE ( 'NONE', *, *, #18639, .F. ) ;
#11539 = ORIENTED_EDGE ( 'NONE', *, *, #9305, .F. ) ;
#11540 = ORIENTED_EDGE ( 'NONE', *, *, #5013, .F. ) ;
#11541 = EDGE_CURVE ( 'NONE', #7335, #21472, #15252, .T. ) ;
#11542 = FACE_OUTER_BOUND ( 'NONE', #1712, .T. ) ;
#11543 = EDGE_CURVE ( 'NONE', #19547, #3082, #20986, .T. ) ;
#11544 = CARTESIAN_POINT ( 'NONE',  ( -30.67540678000428045, 63.74634676501045050, 3.500000000000000000 ) ) ;
#11545 = ORIENTED_EDGE ( 'NONE', *, *, #1158, .F. ) ;
#11546 = EDGE_CURVE ( 'NONE', #9267, #17841, #10272, .T. ) ;
#11547 = CARTESIAN_POINT ( 'NONE',  ( -1.724728116533986721, 42.31054587065082728, 29.66679706732590560 ) ) ;
#11548 = LINE ( 'NONE', #18374, #10430 ) ;
#11549 = DIRECTION ( 'NONE',  ( 0.000000000000000000, 0.000000000000000000, 1.000000000000000000 ) ) ;
#11550 = DIRECTION ( 'NONE',  ( -1.000000000000000000, 0.000000000000000000, 0.000000000000000000 ) ) ;
#11551 = ORIENTED_EDGE ( 'NONE', *, *, #6695, .F. ) ;
#11552 = VERTEX_POINT ( 'NONE', #15445 ) ;
#11553 = EDGE_LOOP ( 'NONE', ( #20036, #10712, #21798, #2958 ) ) ;
#11554 = DIRECTION ( 'NONE',  ( 0.000000000000000000, 0.000000000000000000, 1.000000000000000000 ) ) ;
#11555 = CARTESIAN_POINT ( 'NONE',  ( -1.824728116533986810, 43.31054587065082728, 43.70876104995653577 ) ) ;
#11556 = ADVANCED_FACE ( 'NONE', ( #212 ), #6628, .T. ) ;
#11557 = ORIENTED_EDGE ( 'NONE', *, *, #10908, .T. ) ;
#11558 = CARTESIAN_POINT ( 'NONE',  ( 1.724728116533978728, 43.31054587065082728, 45.71679706732590631 ) ) ;
#11559 = VECTOR ( 'NONE', #1557, 1000.000000000000000 ) ;
#11560 = VERTEX_POINT ( 'NONE', #1681 ) ;
#11561 = EDGE_CURVE ( 'NONE', #19790, #17862, #4622, .T. ) ;
#11562 = DIRECTION ( 'NONE',  ( -0.000000000000000000, -0.000000000000000000, -1.000000000000000000 ) ) ;
#11563 = DIRECTION ( 'NONE',  ( 0.000000000000000000, 0.000000000000000000, -1.000000000000000000 ) ) ;
#11564 = CARTESIAN_POINT ( 'NONE',  ( -15.95292532278785913, -52.11873716947361856, 14.00000000000000000 ) ) ;
#11565 = EDGE_CURVE ( 'NONE', #18107, #15401, #18581, .T. ) ;
#11566 = DIRECTION ( 'NONE',  ( 0.000000000000000000, 0.000000000000000000, 1.000000000000000000 ) ) ;
#11567 = ORIENTED_EDGE ( 'NONE', *, *, #10992, .F. ) ;
#11568 = DIRECTION ( 'NONE',  ( 0.000000000000000000, 0.000000000000000000, 1.000000000000000000 ) ) ;
#11569 = ADVANCED_FACE ( 'NONE', ( #20497 ), #15337, .F. ) ;
#11570 = DIRECTION ( 'NONE',  ( 0.000000000000000000, 1.000000000000000000, 0.000000000000000000 ) ) ;
#11571 = DIRECTION ( 'NONE',  ( 0.000000000000000000, 0.000000000000000000, 1.000000000000000000 ) ) ;
#11572 = DIRECTION ( 'NONE',  ( -0.2309407893632139108, 0.9729678061520308230, 0.000000000000000000 ) ) ;
#11573 = EDGE_LOOP ( 'NONE', ( #2927, #18701, #17807, #21970 ) ) ;
#11574 = ORIENTED_EDGE ( 'NONE', *, *, #2871, .T. ) ;
#11575 = CARTESIAN_POINT ( 'NONE',  ( -8.641460742840918030, -32.93424481021354921, 68.00000000000000000 ) ) ;
#11576 = FACE_OUTER_BOUND ( 'NONE', #2532, .T. ) ;
#11577 = ORIENTED_EDGE ( 'NONE', *, *, #6142, .T. ) ;
#11578 = ORIENTED_EDGE ( 'NONE', *, *, #20353, .F. ) ;
#11579 = VERTEX_POINT ( 'NONE', #13424 ) ;
#11580 = DIRECTION ( 'NONE',  ( -0.000000000000000000, 1.000000000000000000, 0.000000000000000000 ) ) ;
#11581 = DIRECTION ( 'NONE',  ( 1.000000000000000000, 0.000000000000000000, 0.000000000000000000 ) ) ;
#11582 = ORIENTED_EDGE ( 'NONE', *, *, #7197, .T. ) ;
#11583 = CARTESIAN_POINT ( 'NONE',  ( -21.92816239687475743, 42.46645089659918426, 68.25000000000000000 ) ) ;
#11584 = ORIENTED_EDGE ( 'NONE', *, *, #20245, .T. ) ;
#11585 = EDGE_CURVE ( 'NONE', #10953, #18524, #8523, .T. ) ;
#11586 = ORIENTED_EDGE ( 'NONE', *, *, #17439, .T. ) ;
#11587 = DIRECTION ( 'NONE',  ( 0.000000000000000000, 0.000000000000000000, -1.000000000000000000 ) ) ;
#11588 = CARTESIAN_POINT ( 'NONE',  ( -14.83748569039512155, -41.93480993936275780, 13.49999999999999822 ) ) ;
#11589 = CYLINDRICAL_SURFACE ( 'NONE', #6721, 0.2999999999999999334 ) ;
#11590 = DIRECTION ( 'NONE',  ( -1.000000000000000000, 0.000000000000000000, 0.000000000000000000 ) ) ;
#11591 = CIRCLE ( 'NONE', #20185, 0.05000000000000143219 ) ;
#11592 = CARTESIAN_POINT ( 'NONE',  ( 1.774728116533979660, 43.26054587065083012, 47.80876104995653719 ) ) ;
#11593 = CIRCLE ( 'NONE', #10537, 0.04999999999999991257 ) ;
#11594 = FACE_OUTER_BOUND ( 'NONE', #10720, .T. ) ;
#11595 = ADVANCED_FACE ( 'NONE', ( #6861 ), #10194, .F. ) ;
#11596 = LINE ( 'NONE', #1308, #21398 ) ;
#11597 = CARTESIAN_POINT ( 'NONE',  ( -30.79999999999999361, -84.70000000000001705, 0.2999999999999999334 ) ) ;
#11598 = DIRECTION ( 'NONE',  ( -1.000000000000000000, 0.000000000000000000, 0.000000000000000000 ) ) ;
#11599 = ORIENTED_EDGE ( 'NONE', *, *, #3561, .F. ) ;
#11600 = LINE ( 'NONE', #16870, #20564 ) ;
#11601 = CARTESIAN_POINT ( 'NONE',  ( 1.824728116533979705, 42.36054587065083155, 41.66679706732590915 ) ) ;
#11602 = ORIENTED_EDGE ( 'NONE', *, *, #9442, .F. ) ;
#11603 = DIRECTION ( 'NONE',  ( -1.000000000000000000, 0.000000000000000000, 0.000000000000000000 ) ) ;
#11604 = ORIENTED_EDGE ( 'NONE', *, *, #11853, .F. ) ;
#11605 = AXIS2_PLACEMENT_3D ( 'NONE', #5809, #511, #302 ) ;
#11606 = ORIENTED_EDGE ( 'NONE', *, *, #13604, .T. ) ;
#11607 = TOROIDAL_SURFACE ( 'NONE', #14460, 1.750000000000000000, 0.2500000000000000000 ) ;
#11608 = DIRECTION ( 'NONE',  ( -6.123233995736764803E-17, 0.000000000000000000, 1.000000000000000000 ) ) ;
#11609 = ADVANCED_FACE ( 'NONE', ( #18804 ), #20602, .F. ) ;
#11610 = VERTEX_POINT ( 'NONE', #3480 ) ;
#11611 = ADVANCED_FACE ( 'NONE', ( #10316 ), #9560, .T. ) ;
#11612 = DIRECTION ( 'NONE',  ( 1.000000000000000000, -0.000000000000000000, -0.000000000000000000 ) ) ;
#11613 = ORIENTED_EDGE ( 'NONE', *, *, #14641, .F. ) ;
#11614 = DIRECTION ( 'NONE',  ( 8.673617379884034239E-17, 0.000000000000000000, -1.000000000000000000 ) ) ;
#11615 = COLOUR_RGB ( '', 0.09019608, 0.27058824, 0.51372549) ;
#11616 = CARTESIAN_POINT ( 'NONE',  ( 33.79999999999999716, 85.00000000000000000, 1.799999999999996048 ) ) ;
#11617 = DIRECTION ( 'NONE',  ( -0.2309407893631451325, 0.9729678061520472543, 0.000000000000000000 ) ) ;
#11618 = CARTESIAN_POINT ( 'NONE',  ( -18.22752199202934520, 50.11873716947361856, 13.50000000000000000 ) ) ;
#11619 = AXIS2_PLACEMENT_3D ( 'NONE', #5220, #12016, #17178 ) ;
#11620 = VECTOR ( 'NONE', #13597, 1000.000000000000000 ) ;
#11621 = CIRCLE ( 'NONE', #14126, 2.500000000000002220 ) ;
#11622 = DIRECTION ( 'NONE',  ( 0.000000000000000000, 0.000000000000000000, 1.000000000000000000 ) ) ;
#11623 = CARTESIAN_POINT ( 'NONE',  ( 26.61833302554978786, 9.663695060508649348, 13.79999999999999893 ) ) ;
#11624 = DIRECTION ( 'NONE',  ( 0.000000000000000000, 1.000000000000000000, 0.000000000000000000 ) ) ;
#11626 = ADVANCED_FACE ( 'NONE', ( #3259 ), #8400, .T. ) ;
#11625 = CARTESIAN_POINT ( 'NONE',  ( 28.90789898151107451, -6.496209923375007911, 7.643284004395015430 ) ) ;
#11627 = DIRECTION ( 'NONE',  ( 1.000000000000000000, 0.000000000000000000, 0.000000000000000000 ) ) ;
#11628 = ORIENTED_EDGE ( 'NONE', *, *, #11896, .T. ) ;
#11629 = DIRECTION ( 'NONE',  ( 2.832483164223434527E-16, 1.000000000000000000, -0.000000000000000000 ) ) ;
#11630 = AXIS2_PLACEMENT_3D ( 'NONE', #20351, #5361, #5469 ) ;
#11632 = DIRECTION ( 'NONE',  ( 1.000000000000000000, -0.000000000000000000, 0.000000000000000000 ) ) ;
#11631 = TOROIDAL_SURFACE ( 'NONE', #1989, 1.000000000000000000, 0.5000000000000000000 ) ;
#11633 = ORIENTED_EDGE ( 'NONE', *, *, #4274, .F. ) ;
#11634 = CIRCLE ( 'NONE', #17010, 4.193574995607837863 ) ;
#11635 = VERTEX_POINT ( 'NONE', #6963 ) ;
#11636 = DIRECTION ( 'NONE',  ( 1.000000000000000000, -0.000000000000000000, -0.000000000000000000 ) ) ;
#11637 = EDGE_CURVE ( 'NONE', #444, #5889, #11336, .T. ) ;
#11638 = DIRECTION ( 'NONE',  ( 0.000000000000000000, 0.000000000000000000, 1.000000000000000000 ) ) ;
#11639 = EDGE_CURVE ( 'NONE', #9803, #13239, #7068, .T. ) ;
#11640 = ORIENTED_EDGE ( 'NONE', *, *, #11140, .F. ) ;
#11641 = CIRCLE ( 'NONE', #4510, 5.300000000000006040 ) ;
#11642 = EDGE_LOOP ( 'NONE', ( #9876, #1469, #20401, #15836, #5121 ) ) ;
#11643 = ORIENTED_EDGE ( 'NONE', *, *, #15099, .F. ) ;
#11644 = ORIENTED_EDGE ( 'NONE', *, *, #7320, .T. ) ;
#11645 = CARTESIAN_POINT ( 'NONE',  ( -1.724728116533986721, 43.31054587065082728, 47.80876104995653719 ) ) ;
#11646 = CIRCLE ( 'NONE', #3460, 2.000000000000001776 ) ;
#11647 = VECTOR ( 'NONE', #20328, 1000.000000000000000 ) ;
#11648 = PLANE ( 'NONE',  #7465 ) ;
#11649 = VECTOR ( 'NONE', #4811, 1000.000000000000000 ) ;
#11650 = ORIENTED_EDGE ( 'NONE', *, *, #9538, .F. ) ;
#11651 = DIRECTION ( 'NONE',  ( -0.000000000000000000, -1.000000000000000000, -0.000000000000000000 ) ) ;
#11652 = EDGE_CURVE ( 'NONE', #5901, #10741, #5391, .T. ) ;
#11653 = CARTESIAN_POINT ( 'NONE',  ( -23.18284705826593850, 2.947275247953579758, 13.45749238763917610 ) ) ;
#11654 = FACE_OUTER_BOUND ( 'NONE', #11573, .T. ) ;
#11655 = DIRECTION ( 'NONE',  ( -0.000000000000000000, 0.000000000000000000, 1.000000000000000000 ) ) ;
#11656 = TOROIDAL_SURFACE ( 'NONE', #14168, 1.500000000000000000, 0.5000000000000000000 ) ;
#11657 = LINE ( 'NONE', #14908, #4708 ) ;
#11658 = ORIENTED_EDGE ( 'NONE', *, *, #1386, .T. ) ;
#11659 = ORIENTED_EDGE ( 'NONE', *, *, #9935, .T. ) ;
#11660 = ORIENTED_EDGE ( 'NONE', *, *, #49, .T. ) ;
#11661 = FACE_OUTER_BOUND ( 'NONE', #8351, .T. ) ;
#11662 = ADVANCED_FACE ( 'NONE', ( #11859 ), #3151, .T. ) ;
#11663 = CARTESIAN_POINT ( 'NONE',  ( -30.07540678000427548, -6.000000000000000000, 7.500000000000000000 ) ) ;
#11664 = EDGE_CURVE ( 'NONE', #15364, #2605, #3495, .T. ) ;
#11665 = EDGE_LOOP ( 'NONE', ( #6872, #6117, #18671, #3993 ) ) ;
#11666 = ADVANCED_FACE ( 'NONE', ( #3699 ), #433, .F. ) ;
#11667 = CIRCLE ( 'NONE', #951, 0.3000000000000000444 ) ;
#11668 = AXIS2_PLACEMENT_3D ( 'NONE', #15192, #11608, #18445 ) ;
#11669 = TOROIDAL_SURFACE ( 'NONE', #14176, 0.2500000000000000000, 0.2500000000000000000 ) ;
#11670 = CARTESIAN_POINT ( 'NONE',  ( 14.96174975910705918, -51.80685496129632384, 13.81241846611418467 ) ) ;
#11671 = AXIS2_PLACEMENT_3D ( 'NONE', #18096, #14633, #14845 ) ;
#11672 = ORIENTED_EDGE ( 'NONE', *, *, #8618, .F. ) ;
#11673 = DIRECTION ( 'NONE',  ( 0.000000000000000000, 0.000000000000000000, 1.000000000000000000 ) ) ;
#11674 = EDGE_CURVE ( 'NONE', #5502, #17668, #3932, .T. ) ;
#11675 = CARTESIAN_POINT ( 'NONE',  ( 28.57540678000427548, -63.74634676501045050, 13.19999999999999929 ) ) ;
#11676 = CARTESIAN_POINT ( 'NONE',  ( -15.95292532278785913, 50.11873716947361856, 13.79999999999999893 ) ) ;
#11677 = DIRECTION ( 'NONE',  ( -0.000000000000000000, 1.000000000000000000, -0.000000000000000000 ) ) ;
#11678 = ORIENTED_EDGE ( 'NONE', *, *, #20197, .T. ) ;
#11679 = DIRECTION ( 'NONE',  ( -1.000000000000000000, 0.000000000000000000, 0.000000000000000000 ) ) ;
#11680 = CARTESIAN_POINT ( 'NONE',  ( -8.223741455913085474, 41.92645089659918511, 69.94509975324523054 ) ) ;
#11681 = ADVANCED_FACE ( 'NONE', ( #769 ), #13972, .F. ) ;
#11682 = AXIS2_PLACEMENT_3D ( 'NONE', #15778, #3948, #9187 ) ;
#11683 = FACE_OUTER_BOUND ( 'NONE', #7427, .T. ) ;
#11684 = DIRECTION ( 'NONE',  ( -6.123233995736764803E-17, 0.000000000000000000, 1.000000000000000000 ) ) ;
#11685 = DIRECTION ( 'NONE',  ( -1.000000000000000000, 0.000000000000000000, 0.000000000000000000 ) ) ;
#11686 = ORIENTED_EDGE ( 'NONE', *, *, #17867, .F. ) ;
#11687 = CIRCLE ( 'NONE', #2022, 0.9652499999999990532 ) ;
#11688 = AXIS2_PLACEMENT_3D ( 'NONE', #4253, #11403, #16643 ) ;
#11689 = CARTESIAN_POINT ( 'NONE',  ( 0.000000000000000000, -5.299999999999999822, 7.200000000000000178 ) ) ;
#11690 = EDGE_LOOP ( 'NONE', ( #19824, #18810, #2397, #1099 ) ) ;
#11691 = FACE_OUTER_BOUND ( 'NONE', #20178, .T. ) ;
#11692 = AXIS2_PLACEMENT_3D ( 'NONE', #5321, #18956, #3626 ) ;
#11693 = CARTESIAN_POINT ( 'NONE',  ( 30.07540678000427548, 6.000000000000000000, 7.200000000000000178 ) ) ;
#11694 = EDGE_LOOP ( 'NONE', ( #3233, #15429, #10951, #39 ) ) ;
#11695 = VERTEX_POINT ( 'NONE', #14410 ) ;
#11696 = AXIS2_PLACEMENT_3D ( 'NONE', #5998, #11554, #16705 ) ;
#11697 = VERTEX_POINT ( 'NONE', #17456 ) ;
#11698 = CARTESIAN_POINT ( 'NONE',  ( -14.66174975910705136, -51.76873716947361714, 13.80000000000000071 ) ) ;
#11699 = AXIS2_PLACEMENT_3D ( 'NONE', #4111, #17865, #19549 ) ;
#11700 = EDGE_CURVE ( 'NONE', #9461, #5502, #3849, .T. ) ;
#11701 = CARTESIAN_POINT ( 'NONE',  ( -8.641460742840918030, -33.43424481021354921, 68.00000000000000000 ) ) ;
#11702 = EDGE_CURVE ( 'NONE', #3289, #2536, #1694, .T. ) ;
#11703 = EDGE_LOOP ( 'NONE', ( #16580, #8507, #6557, #8353 ) ) ;
#11704 = DIRECTION ( 'NONE',  ( 1.000000000000000000, 0.000000000000000000, 0.000000000000000000 ) ) ;
#11705 = ADVANCED_FACE ( 'NONE', ( #2339 ), #22081, .T. ) ;
#11706 = EDGE_LOOP ( 'NONE', ( #1277, #7084, #12731, #7722 ) ) ;
#11707 = ORIENTED_EDGE ( 'NONE', *, *, #20381, .T. ) ;
#11708 = DIRECTION ( 'NONE',  ( 1.000000000000000000, 0.000000000000000000, 0.000000000000000000 ) ) ;
#11709 = AXIS2_PLACEMENT_3D ( 'NONE', #11054, #17873, #8039 ) ;
#11710 = AXIS2_PLACEMENT_3D ( 'NONE', #6502, #6719, #13298 ) ;
#11711 = DIRECTION ( 'NONE',  ( 0.000000000000000000, 1.000000000000000000, 0.000000000000000000 ) ) ;
#11712 = CARTESIAN_POINT ( 'NONE',  ( -23.02398829872513986, -3.528912754968629439, 13.80000000000000071 ) ) ;
#11713 = FACE_OUTER_BOUND ( 'NONE', #21754, .T. ) ;
#11714 = AXIS2_PLACEMENT_3D ( 'NONE', #11741, #20254, #3023 ) ;
#11715 = VECTOR ( 'NONE', #19389, 1000.000000000000000 ) ;
#11716 = AXIS2_PLACEMENT_3D ( 'NONE', #18884, #17193, #1867 ) ;
#11717 = CARTESIAN_POINT ( 'NONE',  ( 1.724728116533979838, 43.26054587065083012, 29.66679706732590560 ) ) ;
#11718 = ADVANCED_FACE ( 'NONE', ( #17661 ), #16328, .T. ) ;
#11719 = DIRECTION ( 'NONE',  ( 0.000000000000000000, 0.000000000000000000, -1.000000000000000000 ) ) ;
#11720 = ORIENTED_EDGE ( 'NONE', *, *, #18920, .F. ) ;
#11721 = CARTESIAN_POINT ( 'NONE',  ( -3.627054932750481964, -32.61873716947361856, 42.50000000000000000 ) ) ;
#11722 = ADVANCED_FACE ( 'NONE', ( #17565 ), #8848, .T. ) ;
#11723 = CYLINDRICAL_SURFACE ( 'NONE', #16275, 5.000000000000000888 ) ;
#11724 = VECTOR ( 'NONE', #16046, 1000.000000000000000 ) ;
#11725 = CIRCLE ( 'NONE', #8532, 0.5000000000000004441 ) ;
#11726 = ORIENTED_EDGE ( 'NONE', *, *, #17035, .T. ) ;
#11727 = LINE ( 'NONE', #8172, #2815 ) ;
#11728 = DIRECTION ( 'NONE',  ( 0.000000000000000000, -1.000000000000000000, -0.000000000000000000 ) ) ;
#11729 = VERTEX_POINT ( 'NONE', #5503 ) ;
#11730 = AXIS2_PLACEMENT_3D ( 'NONE', #2868, #16160, #6017 ) ;
#11731 = EDGE_LOOP ( 'NONE', ( #5086, #17941, #2262, #19120 ) ) ;
#11732 = AXIS2_PLACEMENT_3D ( 'NONE', #21167, #11072, #1207 ) ;
#11733 = DIRECTION ( 'NONE',  ( 1.000000000000000000, -0.000000000000000000, -0.000000000000000000 ) ) ;
#11734 = VECTOR ( 'NONE', #16874, 1000.000000000000000 ) ;
#11735 = ADVANCED_FACE ( 'NONE', ( #329 ), #14193, .T. ) ;
#11736 = ORIENTED_EDGE ( 'NONE', *, *, #16471, .T. ) ;
#11737 = FACE_OUTER_BOUND ( 'NONE', #14780, .T. ) ;
#11738 = ORIENTED_EDGE ( 'NONE', *, *, #10406, .F. ) ;
#11739 = DIRECTION ( 'NONE',  ( 0.000000000000000000, 0.000000000000000000, 1.000000000000000000 ) ) ;
#11740 = AXIS2_PLACEMENT_3D ( 'NONE', #15835, #19655, #21231 ) ;
#11741 = CARTESIAN_POINT ( 'NONE',  ( 14.96174975910707161, 41.81054587065082728, 68.25000000000000000 ) ) ;
#11742 = DIRECTION ( 'NONE',  ( -1.000000000000000000, -0.000000000000000000, -0.000000000000000000 ) ) ;
#11743 = AXIS2_PLACEMENT_3D ( 'NONE', #5332, #474, #3410 ) ;
#11744 = CYLINDRICAL_SURFACE ( 'NONE', #3191, 3.500000000000003109 ) ;
#11745 = DIRECTION ( 'NONE',  ( 0.000000000000000000, 0.000000000000000000, 1.000000000000000000 ) ) ;
#11746 = EDGE_CURVE ( 'NONE', #4526, #1398, #4919, .T. ) ;
#11747 = DIRECTION ( 'NONE',  ( 0.000000000000000000, -1.000000000000000000, 0.000000000000000000 ) ) ;
#11748 = ADVANCED_FACE ( 'NONE', ( #2458 ), #2771, .T. ) ;
#11749 = CARTESIAN_POINT ( 'NONE',  ( 14.96174975910707161, 41.81054587065082728, 68.25000000000000000 ) ) ;
#11750 = EDGE_CURVE ( 'NONE', #8125, #13130, #21262, .T. ) ;
#11751 = DIRECTION ( 'NONE',  ( -0.000000000000000000, -0.000000000000000000, -1.000000000000000000 ) ) ;
#11752 = DIRECTION ( 'NONE',  ( 0.000000000000000000, -1.000000000000000000, 0.000000000000000000 ) ) ;
#11753 = ORIENTED_EDGE ( 'NONE', *, *, #4762, .F. ) ;
#11754 = CARTESIAN_POINT ( 'NONE',  ( 28.87540678000427619, 0.000000000000000000, 7.799999999999999822 ) ) ;
#11755 = ORIENTED_EDGE ( 'NONE', *, *, #18650, .F. ) ;
#11756 = VERTEX_POINT ( 'NONE', #15863 ) ;
#11757 = CARTESIAN_POINT ( 'NONE',  ( 8.641460742840918030, 32.93424481021354921, 42.50000000000000000 ) ) ;
#11758 = FILL_AREA_STYLE_COLOUR ( '', #21598 ) ;
#11759 = ORIENTED_EDGE ( 'NONE', *, *, #11988, .T. ) ;
#11760 =( NAMED_UNIT ( * ) SI_UNIT ( $, .STERADIAN. ) SOLID_ANGLE_UNIT ( ) );
#11761 = ORIENTED_EDGE ( 'NONE', *, *, #18920, .T. ) ;
#11762 = ORIENTED_EDGE ( 'NONE', *, *, #9076, .T. ) ;
#11763 = DIRECTION ( 'NONE',  ( 0.000000000000000000, -1.000000000000000000, 0.000000000000000000 ) ) ;
#11764 = CARTESIAN_POINT ( 'NONE',  ( 14.66174975910705847, -51.76873716947361004, 13.50000000000000000 ) ) ;
#11765 = DIRECTION ( 'NONE',  ( 0.000000000000000000, 0.000000000000000000, 1.000000000000000000 ) ) ;
#11766 = AXIS2_PLACEMENT_3D ( 'NONE', #14573, #5984, #14352 ) ;
#11767 = CARTESIAN_POINT ( 'NONE',  ( 17.95292532278785913, 0.000000000000000000, 42.50000000000000711 ) ) ;
#11768 = EDGE_LOOP ( 'NONE', ( #2569, #16668, #17049, #5715 ) ) ;
#11769 = EDGE_CURVE ( 'NONE', #341, #10170, #15610, .T. ) ;
#11770 = AXIS2_PLACEMENT_3D ( 'NONE', #8761, #3619, #17355 ) ;
#11771 = LINE ( 'NONE', #30, #15097 ) ;
#11772 = CIRCLE ( 'NONE', #13569, 0.2999999999999999334 ) ;
#11773 = DIRECTION ( 'NONE',  ( 0.000000000000000000, -0.000000000000000000, -1.000000000000000000 ) ) ;
#11774 = LINE ( 'NONE', #6552, #13730 ) ;
#11775 = DIRECTION ( 'NONE',  ( -1.000000000000000000, 0.000000000000000000, 0.000000000000000000 ) ) ;
#11776 = VERTEX_POINT ( 'NONE', #21162 ) ;
#11777 = ORIENTED_EDGE ( 'NONE', *, *, #9399, .T. ) ;
#11778 = ORIENTED_EDGE ( 'NONE', *, *, #16477, .T. ) ;
#11779 = DIRECTION ( 'NONE',  ( 1.734723475976806848E-16, -0.000000000000000000, -1.000000000000000000 ) ) ;
#11780 = CARTESIAN_POINT ( 'NONE',  ( -11.67890639357915816, 42.46645089659918426, 67.85468508031152624 ) ) ;
#11781 = FACE_OUTER_BOUND ( 'NONE', #2303, .T. ) ;
#11782 = VECTOR ( 'NONE', #3858, 1000.000000000000000 ) ;
#11783 = PRODUCT_DEFINITION_SHAPE ( 'NONE', 'NONE',  #19031 ) ;
#11784 = ORIENTED_EDGE ( 'NONE', *, *, #13222, .T. ) ;
#11785 = DIRECTION ( 'NONE',  ( -1.000000000000000000, 0.000000000000000000, 0.000000000000000000 ) ) ;
#11786 = CARTESIAN_POINT ( 'NONE',  ( 3.127054932750481964, -32.61873716947361856, 109.6002446535588319 ) ) ;
#11787 = DIRECTION ( 'NONE',  ( -1.000000000000000000, 0.000000000000000000, 0.000000000000000000 ) ) ;
#11788 = ORIENTED_EDGE ( 'NONE', *, *, #1204, .F. ) ;
#11789 = CYLINDRICAL_SURFACE ( 'NONE', #22049, 0.3000000000000016542 ) ;
#11790 = DIRECTION ( 'NONE',  ( 0.000000000000000000, -0.000000000000000000, -1.000000000000000000 ) ) ;
#11791 = EDGE_CURVE ( 'NONE', #11183, #7362, #5650, .T. ) ;
#11792 = CARTESIAN_POINT ( 'NONE',  ( 17.95292532278785913, 0.000000000000000000, 109.6002446535588319 ) ) ;
#11793 = EDGE_CURVE ( 'NONE', #18174, #11393, #1105, .T. ) ;
#11794 = FACE_OUTER_BOUND ( 'NONE', #2124, .T. ) ;
#11795 = ORIENTED_EDGE ( 'NONE', *, *, #21843, .F. ) ;
#11796 = DIRECTION ( 'NONE',  ( 0.000000000000000000, 0.000000000000000000, -1.000000000000000000 ) ) ;
#11797 = AXIS2_PLACEMENT_3D ( 'NONE', #10857, #4045, #1929 ) ;
#11798 = ORIENTED_EDGE ( 'NONE', *, *, #13752, .F. ) ;
#11799 = AXIS2_PLACEMENT_3D ( 'NONE', #17143, #15462, #131 ) ;
#11800 = DIRECTION ( 'NONE',  ( 0.000000000000000000, 0.000000000000000000, 1.000000000000000000 ) ) ;
#11801 = CARTESIAN_POINT ( 'NONE',  ( -1.724728116533986721, 42.36054587065083155, 53.66679706732590915 ) ) ;
#11802 = ORIENTED_EDGE ( 'NONE', *, *, #19313, .F. ) ;
#11803 = ORIENTED_EDGE ( 'NONE', *, *, #6524, .F. ) ;
#11804 = ORIENTED_EDGE ( 'NONE', *, *, #8754, .F. ) ;
#11805 = EDGE_CURVE ( 'NONE', #16312, #15418, #20656, .T. ) ;
#11806 = CARTESIAN_POINT ( 'NONE',  ( -30.37540678000427619, 0.000000000000000000, 7.500000000000000000 ) ) ;
#11807 = LINE ( 'NONE', #15283, #696 ) ;
#11808 = VERTEX_POINT ( 'NONE', #13190 ) ;
#11809 = CYLINDRICAL_SURFACE ( 'NONE', #624, 0.5000000000000004441 ) ;
#11810 = ADVANCED_FACE ( 'NONE', ( #21606 ), #14857, .T. ) ;
#11811 = VERTEX_POINT ( 'NONE', #4361 ) ;
#11812 = DIRECTION ( 'NONE',  ( 0.000000000000000000, -1.000000000000000000, 3.614007241618411485E-15 ) ) ;
#11813 = ORIENTED_EDGE ( 'NONE', *, *, #3218, .T. ) ;
#11814 = DIRECTION ( 'NONE',  ( 0.000000000000000000, 0.000000000000000000, -1.000000000000000000 ) ) ;
#11815 = AXIS2_PLACEMENT_3D ( 'NONE', #11489, #19673, #20122 ) ;
#11816 = CARTESIAN_POINT ( 'NONE',  ( 25.37540678000426908, 38.74634676501045760, 42.50000000000000000 ) ) ;
#11817 = CARTESIAN_POINT ( 'NONE',  ( -29.69597781366221412, 27.99124249474150972, 70.25000000000000000 ) ) ;
#11818 = CARTESIAN_POINT ( 'NONE',  ( -32.48382792203229741, 83.71979900898287497, 13.74999999999999822 ) ) ;
#11819 = ORIENTED_EDGE ( 'NONE', *, *, #13496, .T. ) ;
#11820 = CARTESIAN_POINT ( 'NONE',  ( 23.02398829872513986, 2.157133568461118589, 13.20000000000007923 ) ) ;
#11821 = DIRECTION ( 'NONE',  ( 0.000000000000000000, 0.000000000000000000, 1.000000000000000000 ) ) ;
#11822 = EDGE_CURVE ( 'NONE', #20447, #488, #18861, .T. ) ;
#11823 = ADVANCED_FACE ( 'NONE', ( #6057 ), #990, .T. ) ;
#11824 = CARTESIAN_POINT ( 'NONE',  ( 14.96174975910705918, 51.86873716947361856, 14.00000000000000000 ) ) ;
#11825 = CYLINDRICAL_SURFACE ( 'NONE', #7839, 0.5000000000000004441 ) ;
#11826 = ORIENTED_EDGE ( 'NONE', *, *, #6116, .F. ) ;
#11827 = DIRECTION ( 'NONE',  ( 1.224646799147353207E-16, 0.000000000000000000, 1.000000000000000000 ) ) ;
#11828 = EDGE_CURVE ( 'NONE', #6444, #14759, #12841, .T. ) ;
#11829 = VECTOR ( 'NONE', #13258, 1000.000000000000000 ) ;
#11830 = CIRCLE ( 'NONE', #15422, 0.2500000000000002220 ) ;
#11831 = EDGE_LOOP ( 'NONE', ( #21499, #21994, #4548, #7190 ) ) ;
#11832 = FACE_OUTER_BOUND ( 'NONE', #11731, .T. ) ;
#11833 = DIRECTION ( 'NONE',  ( -1.000000000000000000, 0.000000000000000000, 0.000000000000000000 ) ) ;
#11834 = CIRCLE ( 'NONE', #19658, 0.2499999999999977796 ) ;
#11835 = ORIENTED_EDGE ( 'NONE', *, *, #9505, .F. ) ;
#11836 = ORIENTED_EDGE ( 'NONE', *, *, #16599, .T. ) ;
#11837 = DIRECTION ( 'NONE',  ( 1.000000000000000000, 0.000000000000000000, 0.000000000000000000 ) ) ;
#11838 = EDGE_CURVE ( 'NONE', #17988, #6219, #12397, .T. ) ;
#11839 = CIRCLE ( 'NONE', #15057, 2.500000000000002220 ) ;
#11840 = EDGE_LOOP ( 'NONE', ( #14532, #10155, #8230, #12040 ) ) ;
#11841 = AXIS2_PLACEMENT_3D ( 'NONE', #12801, #19649, #11234 ) ;
#11842 = CIRCLE ( 'NONE', #13638, 1.984122918275925462 ) ;
#11843 = DIRECTION ( 'NONE',  ( 2.107255972849994642E-16, -0.000000000000000000, 1.000000000000000000 ) ) ;
#11844 = EDGE_LOOP ( 'NONE', ( #17073, #4079 ) ) ;
#11845 = CARTESIAN_POINT ( 'NONE',  ( -29.44760963940965226, 2.533475775848048617, 0.1250376690123979340 ) ) ;
#11846 = AXIS2_PLACEMENT_3D ( 'NONE', #36, #20632, #21978 ) ;
#11847 = CARTESIAN_POINT ( 'NONE',  ( -1.824728116533986810, 43.26054587065083012, 43.80876104995653719 ) ) ;
#11848 = DIRECTION ( 'NONE',  ( 0.000000000000000000, 0.000000000000000000, 1.000000000000000000 ) ) ;
#11849 = DIRECTION ( 'NONE',  ( -1.000000000000000000, -0.000000000000000000, -4.336808689942194441E-15 ) ) ;
#11850 = EDGE_CURVE ( 'NONE', #6556, #1070, #18479, .T. ) ;
#11851 = CARTESIAN_POINT ( 'NONE',  ( 0.000000000000000000, 51.61873716947361856, 68.00000000000000000 ) ) ;
#11852 = LINE ( 'NONE', #18687, #8261 ) ;
#11853 = EDGE_CURVE ( 'NONE', #9625, #21235, #19920, .T. ) ;
#11854 = DIRECTION ( 'NONE',  ( 0.000000000000000000, 0.000000000000000000, 1.000000000000000000 ) ) ;
#11855 = DIRECTION ( 'NONE',  ( 1.000000000000000000, 0.000000000000000000, 0.000000000000000000 ) ) ;
#11856 = DIRECTION ( 'NONE',  ( -0.000000000000000000, -0.000000000000000000, -1.000000000000000000 ) ) ;
#11857 = ORIENTED_EDGE ( 'NONE', *, *, #2779, .F. ) ;
#11858 = CIRCLE ( 'NONE', #14720, 0.9652499999999990532 ) ;
#11859 = FACE_OUTER_BOUND ( 'NONE', #7594, .T. ) ;
#11860 = ORIENTED_EDGE ( 'NONE', *, *, #19331, .F. ) ;
#11861 = CARTESIAN_POINT ( 'NONE',  ( -1.724728116533986721, 43.31054587065082728, 43.80876104995653719 ) ) ;
#11862 = AXIS2_PLACEMENT_3D ( 'NONE', #19448, #21367, #10942 ) ;
#11863 = VERTEX_POINT ( 'NONE', #21825 ) ;
#11864 = VERTEX_POINT ( 'NONE', #19689 ) ;
#11865 = CARTESIAN_POINT ( 'NONE',  ( 0.000000000000000000, 68.70000000000001705, 0.2999999999999947153 ) ) ;
#11866 = DIRECTION ( 'NONE',  ( 0.000000000000000000, 0.000000000000000000, 1.000000000000000000 ) ) ;
#11867 = VERTEX_POINT ( 'NONE', #2568 ) ;
#11868 = ADVANCED_FACE ( 'NONE', ( #18231 ), #2792, .T. ) ;
#11869 = ORIENTED_EDGE ( 'NONE', *, *, #1542, .T. ) ;
#11870 = EDGE_CURVE ( 'NONE', #381, #8599, #16702, .T. ) ;
#11871 = ORIENTED_EDGE ( 'NONE', *, *, #49, .F. ) ;
#11872 = AXIS2_PLACEMENT_3D ( 'NONE', #867, #21603, #9393 ) ;
#11873 = CARTESIAN_POINT ( 'NONE',  ( -25.37540678000426908, 38.74634676501045760, 42.50000000000000000 ) ) ;
#11874 = CARTESIAN_POINT ( 'NONE',  ( -1.724728116533986721, 43.31054587065082728, 31.80876104995653719 ) ) ;
#11875 = CARTESIAN_POINT ( 'NONE',  ( 0.000000000000000000, -52.11873716947361856, 68.00000000000000000 ) ) ;
#11876 = ORIENTED_EDGE ( 'NONE', *, *, #14736, .F. ) ;
#11877 = EDGE_CURVE ( 'NONE', #5205, #8641, #1336, .T. ) ;
#11878 = CARTESIAN_POINT ( 'NONE',  ( -23.32398829872514057, 3.528912754968630328, 13.50000000000000000 ) ) ;
#11879 = DIRECTION ( 'NONE',  ( -0.000000000000000000, -0.000000000000000000, -1.000000000000000000 ) ) ;
#11880 = CARTESIAN_POINT ( 'NONE',  ( -28.87540678000427263, 6.494748934539262386, 7.720760203330568672 ) ) ;
#11881 = DIRECTION ( 'NONE',  ( 0.000000000000000000, 0.000000000000000000, 1.000000000000000000 ) ) ;
#11882 = VECTOR ( 'NONE', #6983, 1000.000000000000000 ) ;
#11883 = DIRECTION ( 'NONE',  ( -1.000000000000000000, 0.000000000000000000, 0.000000000000000000 ) ) ;
#11884 = ORIENTED_EDGE ( 'NONE', *, *, #12062, .F. ) ;
#11885 = ORIENTED_EDGE ( 'NONE', *, *, #6818, .F. ) ;
#11886 = ORIENTED_EDGE ( 'NONE', *, *, #2014, .F. ) ;
#11887 = DIRECTION ( 'NONE',  ( 0.000000000000000000, 0.000000000000000000, 1.000000000000000000 ) ) ;
#11888 =( NAMED_UNIT ( * ) PLANE_ANGLE_UNIT ( ) SI_UNIT ( $, .RADIAN. ) );
#11889 = CARTESIAN_POINT ( 'NONE',  ( 1.724728116533979616, 42.31054587065082728, 39.75876104995653293 ) ) ;
#11890 = VERTEX_POINT ( 'NONE', #1319 ) ;
#11891 = FACE_OUTER_BOUND ( 'NONE', #14228, .T. ) ;
#11892 = ORIENTED_EDGE ( 'NONE', *, *, #4115, .F. ) ;
#11893 = EDGE_CURVE ( 'NONE', #14859, #15917, #2040, .T. ) ;
#11894 = EDGE_LOOP ( 'NONE', ( #9339, #16720, #13425, #17080 ) ) ;
#11895 = CARTESIAN_POINT ( 'NONE',  ( 15.95292532278785913, 51.61873716947361856, 14.00000000000000000 ) ) ;
#11896 = EDGE_CURVE ( 'NONE', #21952, #6609, #7718, .T. ) ;
#11897 = CARTESIAN_POINT ( 'NONE',  ( -1.724728116533986721, 43.26054587065083012, 27.80876104995653719 ) ) ;
#11898 = DIRECTION ( 'NONE',  ( 0.000000000000000000, 0.000000000000000000, 1.000000000000000000 ) ) ;
#11899 = VERTEX_POINT ( 'NONE', #9394 ) ;
#11900 = FACE_OUTER_BOUND ( 'NONE', #14530, .T. ) ;
#11901 = DIRECTION ( 'NONE',  ( -0.000000000000000000, 1.000000000000000000, 0.000000000000000000 ) ) ;
#11902 = CARTESIAN_POINT ( 'NONE',  ( 27.37540678000426908, 36.74634676501047181, 42.50000000000000000 ) ) ;
#11903 = CARTESIAN_POINT ( 'NONE',  ( 14.96174975910707161, -51.61873716947361856, 68.00000000000000000 ) ) ;
#11904 = DIRECTION ( 'NONE',  ( -1.000000000000000000, 0.000000000000000000, 0.000000000000000000 ) ) ;
#11905 = VERTEX_POINT ( 'NONE', #21378 ) ;
#11906 = CARTESIAN_POINT ( 'NONE',  ( 1.724728116533979838, 43.31054587065082728, 53.71679706732590631 ) ) ;
#11907 = ORIENTED_EDGE ( 'NONE', *, *, #19073, .F. ) ;
#11908 = FACE_OUTER_BOUND ( 'NONE', #11334, .T. ) ;
#11909 = DIRECTION ( 'NONE',  ( -1.000000000000000000, 0.000000000000000000, 0.000000000000000000 ) ) ;
#11910 = DIRECTION ( 'NONE',  ( -0.000000000000000000, 1.000000000000000000, -0.000000000000000000 ) ) ;
#11911 = EDGE_CURVE ( 'NONE', #4141, #2085, #6168, .T. ) ;
#11912 = EDGE_LOOP ( 'NONE', ( #14487, #14088, #661, #17368, #16082, #17227, #4321, #6629 ) ) ;
#11913 = VERTEX_POINT ( 'NONE', #16194 ) ;
#11914 = ORIENTED_EDGE ( 'NONE', *, *, #865, .F. ) ;
#11915 = CARTESIAN_POINT ( 'NONE',  ( 15.95292532278785913, -50.11873716947361856, 13.79999999999999893 ) ) ;
#11916 = DIRECTION ( 'NONE',  ( 0.000000000000000000, 0.000000000000000000, -1.000000000000000000 ) ) ;
#11917 = CARTESIAN_POINT ( 'NONE',  ( -12.92890639357915816, 42.46645089659918426, 67.85468508031152624 ) ) ;
#11918 = STYLED_ITEM ( 'NONE', ( #15893 ), #7272 ) ;
#11919 = ORIENTED_EDGE ( 'NONE', *, *, #5153, .T. ) ;
#11920 = ADVANCED_FACE ( 'NONE', ( #869, #18106 ), #9627, .F. ) ;
#11921 = EDGE_CURVE ( 'NONE', #11695, #1150, #101, .T. ) ;
#11922 = ORIENTED_EDGE ( 'NONE', *, *, #9251, .F. ) ;
#11923 = CARTESIAN_POINT ( 'NONE',  ( -29.37540678000427619, -6.000000000000000000, 3.500000000000000000 ) ) ;
#11924 = AXIS2_PLACEMENT_3D ( 'NONE', #7148, #13943, #10597 ) ;
#11925 = ORIENTED_EDGE ( 'NONE', *, *, #14319, .T. ) ;
#11926 = CARTESIAN_POINT ( 'NONE',  ( -23.32398829872514057, -3.528912754968629439, 13.50000000000000178 ) ) ;
#11927 = CARTESIAN_POINT ( 'NONE',  ( -1.724728116533986721, 42.36054587065083155, 33.71679706732589921 ) ) ;
#11928 = CARTESIAN_POINT ( 'NONE',  ( -9.178906393579156386, 42.46645089659917716, 68.50000000000000000 ) ) ;
#11929 = DIRECTION ( 'NONE',  ( 1.224646799147353207E-16, 0.000000000000000000, 1.000000000000000000 ) ) ;
#11930 = EDGE_LOOP ( 'NONE', ( #4474, #17741, #1375, #8413 ) ) ;
#11931 = FACE_OUTER_BOUND ( 'NONE', #21854, .T. ) ;
#11932 = CIRCLE ( 'NONE', #11206, 4.351418481279133665 ) ;
#11933 = CARTESIAN_POINT ( 'NONE',  ( -1.774728116533986544, 43.31054587065082728, 27.80876104995653719 ) ) ;
#11934 = CARTESIAN_POINT ( 'NONE',  ( -31.50000000000002132, 71.00000000000001421, 3.200000000000000178 ) ) ;
#11935 = PRODUCT_DEFINITION_FORMATION_WITH_SPECIFIED_SOURCE ( 'ANY', '', #6454, .NOT_KNOWN. ) ;
#11936 = ORIENTED_EDGE ( 'NONE', *, *, #15438, .T. ) ;
#11937 = CARTESIAN_POINT ( 'NONE',  ( 14.71174975910707161, 51.61873716947361856, 68.00000000000000000 ) ) ;
#11938 = AXIS2_PLACEMENT_3D ( 'NONE', #10131, #15268, #15050 ) ;
#11939 = ADVANCED_FACE ( 'NONE', ( #3344 ), #13141, .T. ) ;
#11940 = LINE ( 'NONE', #9950, #1264 ) ;
#11941 = ORIENTED_EDGE ( 'NONE', *, *, #17702, .F. ) ;
#11942 = LINE ( 'NONE', #17107, #21401 ) ;
#11943 = DIRECTION ( 'NONE',  ( 0.000000000000000000, 0.000000000000000000, 1.000000000000000000 ) ) ;
#11944 = ORIENTED_EDGE ( 'NONE', *, *, #14108, .F. ) ;
#11945 = DIRECTION ( 'NONE',  ( 0.000000000000000000, 0.000000000000000000, 1.000000000000000000 ) ) ;
#11946 = EDGE_CURVE ( 'NONE', #18991, #20665, #6839, .T. ) ;
#11947 = EDGE_CURVE ( 'NONE', #16130, #7436, #17086, .T. ) ;
#11948 = ORIENTED_EDGE ( 'NONE', *, *, #960, .T. ) ;
#11949 = TOROIDAL_SURFACE ( 'NONE', #16953, 5.193574995607837863, 1.000000000000000000 ) ;
#11950 = DIRECTION ( 'NONE',  ( 0.000000000000000000, 0.000000000000000000, 1.000000000000000000 ) ) ;
#11951 = ORIENTED_EDGE ( 'NONE', *, *, #5817, .F. ) ;
#11952 = DIRECTION ( 'NONE',  ( -1.000000000000000000, 0.000000000000000000, 0.000000000000000000 ) ) ;
#11953 = DIRECTION ( 'NONE',  ( 0.000000000000000000, -1.000000000000000000, 0.000000000000000000 ) ) ;
#11954 = CARTESIAN_POINT ( 'NONE',  ( -31.50000000000002132, -71.00000000000001421, 1.800000000000000044 ) ) ;
#11955 = LINE ( 'NONE', #22163, #15574 ) ;
#11956 = DIRECTION ( 'NONE',  ( -1.224646799147353207E-16, -0.000000000000000000, -1.000000000000000000 ) ) ;
#11957 = CARTESIAN_POINT ( 'NONE',  ( 15.21174975910705918, 41.81054587065082728, 13.50000000000000000 ) ) ;
#11958 = EDGE_CURVE ( 'NONE', #5997, #19359, #8380, .T. ) ;
#11959 = FACE_OUTER_BOUND ( 'NONE', #7995, .T. ) ;
#11960 = CARTESIAN_POINT ( 'NONE',  ( -29.37540678000427619, -5.299999999999999822, 7.500000000000000000 ) ) ;
#11961 = CIRCLE ( 'NONE', #11605, 0.05000000000000143219 ) ;
#11962 = CIRCLE ( 'NONE', #16985, 0.9652499999999990532 ) ;
#11963 = ORIENTED_EDGE ( 'NONE', *, *, #19862, .T. ) ;
#11964 = DIRECTION ( 'NONE',  ( -1.000000000000000000, 0.000000000000000000, 0.000000000000000000 ) ) ;
#11965 = LINE ( 'NONE', #1459, #5967 ) ;
#11966 = ORIENTED_EDGE ( 'NONE', *, *, #21797, .T. ) ;
#11967 = EDGE_LOOP ( 'NONE', ( #19782, #20099, #7159, #2287 ) ) ;
#11968 = DIRECTION ( 'NONE',  ( 0.000000000000000000, 0.000000000000000000, 1.000000000000000000 ) ) ;
#11969 = CARTESIAN_POINT ( 'NONE',  ( 18.35781278715831633, 0.000000000000000000, 0.000000000000000000 ) ) ;
#11970 = EDGE_CURVE ( 'NONE', #5130, #12408, #3139, .T. ) ;
#11971 = ORIENTED_EDGE ( 'NONE', *, *, #18680, .F. ) ;
#11972 = ADVANCED_FACE ( 'NONE', ( #3455 ), #8276, .F. ) ;
#11973 = EDGE_CURVE ( 'NONE', #1975, #8082, #15630, .T. ) ;
#11974 = VERTEX_POINT ( 'NONE', #18441 ) ;
#11975 = TOROIDAL_SURFACE ( 'NONE', #4479, 0.05000000000000000278, 0.05000000000000000278 ) ;
#11976 = CIRCLE ( 'NONE', #4131, 0.05000000000000143219 ) ;
#11977 = AXIS2_PLACEMENT_3D ( 'NONE', #13391, #15411, #15300 ) ;
#11978 = ORIENTED_EDGE ( 'NONE', *, *, #15767, .F. ) ;
#11979 = CARTESIAN_POINT ( 'NONE',  ( 25.37540678000427263, 67.24634676501045760, 7.799999999999999822 ) ) ;
#11980 = DIRECTION ( 'NONE',  ( 1.000000000000000000, -0.000000000000000000, 0.000000000000000000 ) ) ;
#11981 = CARTESIAN_POINT ( 'NONE',  ( -21.92816239687475743, 42.46645089659918426, 68.50000000000000000 ) ) ;
#11982 = CARTESIAN_POINT ( 'NONE',  ( -29.13662752439705272, 5.299999999999999822, 7.200000000000000178 ) ) ;
#11983 = CARTESIAN_POINT ( 'NONE',  ( -17.95292532278785913, 34.11873716947361856, 42.50000000000000711 ) ) ;
#11984 = DIRECTION ( 'NONE',  ( -1.000000000000000000, 0.000000000000000000, 0.000000000000000000 ) ) ;
#11985 = DIRECTION ( 'NONE',  ( 0.000000000000000000, 0.000000000000000000, 1.000000000000000000 ) ) ;
#11986 = CYLINDRICAL_SURFACE ( 'NONE', #9276, 0.5000000000000004441 ) ;
#11987 = CIRCLE ( 'NONE', #16635, 0.04999999999999991257 ) ;
#11988 = EDGE_CURVE ( 'NONE', #13680, #21291, #11004, .T. ) ;
#11989 = PLANE ( 'NONE',  #9729 ) ;
#11990 = CIRCLE ( 'NONE', #14495, 0.2500000000000002220 ) ;
#11991 = ORIENTED_EDGE ( 'NONE', *, *, #14359, .F. ) ;
#11992 = VECTOR ( 'NONE', #17822, 1000.000000000000000 ) ;
#11993 = VECTOR ( 'NONE', #17495, 1000.000000000000000 ) ;
#11994 = ORIENTED_EDGE ( 'NONE', *, *, #1493, .T. ) ;
#11995 = CARTESIAN_POINT ( 'NONE',  ( 30.67540678000428045, -6.000000000000000000, 3.500000000000000000 ) ) ;
#11996 = DIRECTION ( 'NONE',  ( -0.000000000000000000, 1.000000000000000000, -0.000000000000000000 ) ) ;
#11997 = ORIENTED_EDGE ( 'NONE', *, *, #18318, .F. ) ;
#11998 = PLANE ( 'NONE',  #6311 ) ;
#11999 = ADVANCED_FACE ( 'NONE', ( #13634 ), #16875, .F. ) ;
#12000 = DIRECTION ( 'NONE',  ( 0.000000000000000000, 0.000000000000000000, -1.000000000000000000 ) ) ;
#12001 = AXIS2_PLACEMENT_3D ( 'NONE', #21125, #11032, #2419 ) ;
#12002 = CARTESIAN_POINT ( 'NONE',  ( -30.79999999999999005, 69.70000000000001705, 2.571758278209448859E-16 ) ) ;
#12003 = DIRECTION ( 'NONE',  ( 0.000000000000000000, 0.000000000000000000, 1.000000000000000000 ) ) ;
#12004 = LINE ( 'NONE', #16719, #8447 ) ;
#12005 = CIRCLE ( 'NONE', #19175, 4.351418481279137218 ) ;
#12006 = EDGE_LOOP ( 'NONE', ( #1065, #6903, #19373, #20271, #20313, #19666, #2206, #6543 ) ) ;
#12007 = DIRECTION ( 'NONE',  ( -0.000000000000000000, 1.000000000000000000, -0.000000000000000000 ) ) ;
#12008 = DIRECTION ( 'NONE',  ( 0.000000000000000000, 0.000000000000000000, 1.000000000000000000 ) ) ;
#12009 = FACE_OUTER_BOUND ( 'NONE', #2263, .T. ) ;
#12010 = CARTESIAN_POINT ( 'NONE',  ( -9.178906393579156386, 42.46645089659917716, 69.50000000000000000 ) ) ;
#12011 = DIRECTION ( 'NONE',  ( -0.000000000000000000, 1.000000000000000000, -0.000000000000000000 ) ) ;
#12012 = CARTESIAN_POINT ( 'NONE',  ( -14.96174975910705207, 51.76873716947361714, 13.79999999999999716 ) ) ;
#12013 = EDGE_CURVE ( 'NONE', #10473, #1026, #21377, .T. ) ;
#12014 = ORIENTED_EDGE ( 'NONE', *, *, #18971, .F. ) ;
#12015 = DIRECTION ( 'NONE',  ( -6.123233995736764803E-17, 0.000000000000000000, 1.000000000000000000 ) ) ;
#12016 = DIRECTION ( 'NONE',  ( -0.000000000000000000, 0.000000000000000000, 1.000000000000000000 ) ) ;
#12017 = FACE_OUTER_BOUND ( 'NONE', #9682, .T. ) ;
#12018 = EDGE_CURVE ( 'NONE', #1177, #5916, #1355, .T. ) ;
#12019 = CIRCLE ( 'NONE', #17742, 0.04999999999999991257 ) ;
#12020 = ORIENTED_EDGE ( 'NONE', *, *, #2295, .F. ) ;
#12021 = CIRCLE ( 'NONE', #2375, 1.162443609680678280 ) ;
#12022 = AXIS2_PLACEMENT_3D ( 'NONE', #20443, #16734, #5111 ) ;
#12023 = VERTEX_POINT ( 'NONE', #18903 ) ;
#12024 = EDGE_LOOP ( 'NONE', ( #21289, #11539, #18718, #11348 ) ) ;
#12025 = DIRECTION ( 'NONE',  ( 0.000000000000000000, 0.000000000000000000, 1.000000000000000000 ) ) ;
#12026 = LINE ( 'NONE', #20669, #20670 ) ;
#12027 = DIRECTION ( 'NONE',  ( 0.000000000000000000, 0.000000000000000000, 1.000000000000000000 ) ) ;
#12028 = CIRCLE ( 'NONE', #14512, 0.5000000000000004441 ) ;
#12029 = ORIENTED_EDGE ( 'NONE', *, *, #9427, .F. ) ;
#12030 = DIRECTION ( 'NONE',  ( 5.464346504236778158E-17, -0.8949343913984425525, 0.4461977533474361102 ) ) ;
#12031 = ORIENTED_EDGE ( 'NONE', *, *, #8562, .T. ) ;
#12032 = CARTESIAN_POINT ( 'NONE',  ( -23.20993114852232964, -3.065002284660066412, 13.47295189337462418 ) ) ;
#12033 = VECTOR ( 'NONE', #18598, 1000.000000000000000 ) ;
#12034 = CARTESIAN_POINT ( 'NONE',  ( -15.95292532278785913, 51.61873716947361856, 68.50000000000000000 ) ) ;
#12035 = ADVANCED_FACE ( 'NONE', ( #15425 ), #17211, .T. ) ;
#12036 = AXIS2_PLACEMENT_3D ( 'NONE', #14764, #13200, #14651 ) ;
#12037 = AXIS2_PLACEMENT_3D ( 'NONE', #10420, #6746, #16788 ) ;
#12038 = DIRECTION ( 'NONE',  ( 1.000000000000000000, 0.000000000000000000, 0.000000000000000000 ) ) ;
#12039 = DIRECTION ( 'NONE',  ( 0.000000000000000000, 0.000000000000000000, 1.000000000000000000 ) ) ;
#12040 = ORIENTED_EDGE ( 'NONE', *, *, #12652, .T. ) ;
#12041 = CARTESIAN_POINT ( 'NONE',  ( 23.02398829872514696, 2.334736181298144864, 13.36928379767489616 ) ) ;
#12042 = CARTESIAN_POINT ( 'NONE',  ( 15.95292532278785913, -34.11873716947361856, 42.50000000000000711 ) ) ;
#12043 = CONICAL_SURFACE ( 'NONE', #4603, 0.9652499999999990532, 0.06981317007976590994 ) ;
#12044 = LINE ( 'NONE', #6938, #13812 ) ;
#12045 = CARTESIAN_POINT ( 'NONE',  ( -1.824728116533986810, 43.31054587065082728, 39.70876104995653577 ) ) ;
#12046 = ORIENTED_EDGE ( 'NONE', *, *, #19114, .T. ) ;
#12047 = CARTESIAN_POINT ( 'NONE',  ( -29.37540678000427619, 6.000000000000000000, 3.500000000000000000 ) ) ;
#12048 = ADVANCED_FACE ( 'NONE', ( #10401 ), #19591, .T. ) ;
#12049 = DIRECTION ( 'NONE',  ( 1.000000000000000000, 0.000000000000000000, 0.000000000000000000 ) ) ;
#12050 = ORIENTED_EDGE ( 'NONE', *, *, #11652, .F. ) ;
#12051 = CARTESIAN_POINT ( 'NONE',  ( -29.69597781366221767, 56.94165929845684815, 70.50000000000000000 ) ) ;
#12052 = DIRECTION ( 'NONE',  ( 0.000000000000000000, 0.000000000000000000, -1.000000000000000000 ) ) ;
#12053 = CIRCLE ( 'NONE', #5296, 2.800000000000003819 ) ;
#12054 = VECTOR ( 'NONE', #524, 1000.000000000000000 ) ;
#12055 = AXIS2_PLACEMENT_3D ( 'NONE', #19573, #16306, #13064 ) ;
#12056 = ORIENTED_EDGE ( 'NONE', *, *, #1043, .F. ) ;
#12057 = LINE ( 'NONE', #6947, #18478 ) ;
#12058 = B_SPLINE_CURVE_WITH_KNOTS ( 'NONE', 3,
 ( #10088, #16898, #11420, #11526 ),
 .UNSPECIFIED., .F., .F.,
 ( 4, 4 ),
 ( 0.001759598105097497350, 0.004588913567995311395 ),
 .UNSPECIFIED. ) ;
#12059 = AXIS2_PLACEMENT_3D ( 'NONE', #16039, #7342, #2185 ) ;
#12060 = ORIENTED_EDGE ( 'NONE', *, *, #18027, .F. ) ;
#12061 = AXIS2_PLACEMENT_3D ( 'NONE', #1489, #15135, #6778 ) ;
#12062 = EDGE_CURVE ( 'NONE', #13130, #2670, #19956, .T. ) ;
#12063 = DIRECTION ( 'NONE',  ( 0.000000000000000000, -1.000000000000000000, -0.000000000000000000 ) ) ;
#12064 = ORIENTED_EDGE ( 'NONE', *, *, #12900, .F. ) ;
#12065 = DIRECTION ( 'NONE',  ( -0.000000000000000000, -0.000000000000000000, -1.000000000000000000 ) ) ;
#12066 = CARTESIAN_POINT ( 'NONE',  ( -34.39999999999999858, -84.70000000000001705, 3.673940397442079220E-17 ) ) ;
#12067 = DIRECTION ( 'NONE',  ( -0.000000000000000000, -0.000000000000000000, -1.000000000000000000 ) ) ;
#12068 = AXIS2_PLACEMENT_3D ( 'NONE', #10151, #18652, #20458 ) ;
#12069 = CARTESIAN_POINT ( 'NONE',  ( -30.49999999999999289, -84.70000000000001705, 0.2999999999999999334 ) ) ;
#12070 = EDGE_CURVE ( 'NONE', #897, #6536, #3239, .T. ) ;
#12071 = DIRECTION ( 'NONE',  ( 0.000000000000000000, 0.000000000000000000, -1.000000000000000000 ) ) ;
#12072 = EDGE_CURVE ( 'NONE', #17577, #8891, #15992, .T. ) ;
#12073 = CIRCLE ( 'NONE', #18147, 1.000000000000000888 ) ;
#12074 = CARTESIAN_POINT ( 'NONE',  ( -1.724728116533986721, 43.31054587065082728, 37.66679706732590915 ) ) ;
#12075 = AXIS2_PLACEMENT_3D ( 'NONE', #8432, #15892, #20748 ) ;
#12076 = AXIS2_PLACEMENT_3D ( 'NONE', #7029, #16965, #8478 ) ;
#12077 = ORIENTED_EDGE ( 'NONE', *, *, #5363, .T. ) ;
#12078 = DIRECTION ( 'NONE',  ( 0.000000000000000000, 0.000000000000000000, -1.000000000000000000 ) ) ;
#12079 = CARTESIAN_POINT ( 'NONE',  ( 1.774728116533979438, 43.31054587065082728, 27.80876104995653719 ) ) ;
#12080 = DIRECTION ( 'NONE',  ( 0.000000000000000000, 1.000000000000000000, 0.000000000000000000 ) ) ;
#12081 = DIRECTION ( 'NONE',  ( 0.000000000000000000, -1.000000000000000000, 0.000000000000000000 ) ) ;
#12082 = ORIENTED_EDGE ( 'NONE', *, *, #8567, .T. ) ;
#12083 = ORIENTED_EDGE ( 'NONE', *, *, #8192, .T. ) ;
#12084 = LINE ( 'NONE', #10638, #13863 ) ;
#12085 = DIRECTION ( 'NONE',  ( 0.000000000000000000, 0.000000000000000000, 1.000000000000000000 ) ) ;
#12086 = ORIENTED_EDGE ( 'NONE', *, *, #8847, .F. ) ;
#12087 = AXIS2_PLACEMENT_3D ( 'NONE', #1429, #14969, #4795 ) ;
#12088 = VERTEX_POINT ( 'NONE', #2214 ) ;
#12089 = EDGE_CURVE ( 'NONE', #2136, #9870, #12491, .T. ) ;
#12090 = CARTESIAN_POINT ( 'NONE',  ( 23.02398829872513986, -2.876860926786022787, 13.71498478227960227 ) ) ;
#12091 = ORIENTED_EDGE ( 'NONE', *, *, #13496, .F. ) ;
#12092 = AXIS2_PLACEMENT_3D ( 'NONE', #10157, #6710, #16973 ) ;
#12093 = VERTEX_POINT ( 'NONE', #21025 ) ;
#12094 = AXIS2_PLACEMENT_3D ( 'NONE', #3238, #1434, #3009 ) ;
#12095 = DIRECTION ( 'NONE',  ( 1.000000000000000000, 0.000000000000000000, 0.000000000000000000 ) ) ;
#12096 = CYLINDRICAL_SURFACE ( 'NONE', #5992, 0.5000000000000004441 ) ;
#12097 = CARTESIAN_POINT ( 'NONE',  ( 23.02398829872513986, 2.279713943076942417, 13.43059441564925116 ) ) ;
#12098 = DIRECTION ( 'NONE',  ( -1.000000000000000000, 0.000000000000000000, 0.000000000000000000 ) ) ;
#12099 = EDGE_CURVE ( 'NONE', #16241, #4674, #1979, .T. ) ;
#12100 = CARTESIAN_POINT ( 'NONE',  ( 3.127054932750481964, 32.61873716947361856, 68.50000000000000000 ) ) ;
#12101 = ADVANCED_FACE ( 'NONE', ( #7267 ), #9047, .F. ) ;
#12102 = LINE ( 'NONE', #15465, #19008 ) ;
#12103 = VECTOR ( 'NONE', #1098, 1000.000000000000000 ) ;
#12104 = CARTESIAN_POINT ( 'NONE',  ( 30.37540678000427619, -6.000000000000000000, 7.200000000000000178 ) ) ;
#12105 = FACE_OUTER_BOUND ( 'NONE', #14525, .T. ) ;
#12106 = EDGE_CURVE ( 'NONE', #19588, #17808, #8827, .T. ) ;
#12107 = DIRECTION ( 'NONE',  ( 0.000000000000000000, 0.000000000000000000, 1.000000000000000000 ) ) ;
#12108 = AXIS2_PLACEMENT_3D ( 'NONE', #8893, #7116, #15698 ) ;
#12109 = EDGE_LOOP ( 'NONE', ( #14705, #6962, #10449, #599 ) ) ;
#12110 = VERTEX_POINT ( 'NONE', #17312 ) ;
#12111 = CARTESIAN_POINT ( 'NONE',  ( 17.45292532278785913, 50.11873716947361856, 68.50000000000000000 ) ) ;
#12112 = CARTESIAN_POINT ( 'NONE',  ( 3.127054932750481964, -33.43424481021354921, 68.50000000000000000 ) ) ;
#12113 = ORIENTED_EDGE ( 'NONE', *, *, #13222, .F. ) ;
#12114 = EDGE_CURVE ( 'NONE', #13197, #4860, #19572, .T. ) ;
#12115 = DIRECTION ( 'NONE',  ( 1.000000000000000000, 0.000000000000000000, 0.000000000000000000 ) ) ;
#12116 = FACE_OUTER_BOUND ( 'NONE', #18332, .T. ) ;
#12117 = TOROIDAL_SURFACE ( 'NONE', #18553, 0.7000000000000000666, 0.2999999999999999889 ) ;
#12118 = CARTESIAN_POINT ( 'NONE',  ( -23.36078716634399655, 44.83461903493144973, 68.50000000000000000 ) ) ;
#12119 = ORIENTED_EDGE ( 'NONE', *, *, #2948, .T. ) ;
#12120 = CARTESIAN_POINT ( 'NONE',  ( -9.641460742840918030, -32.61873716947361856, 68.00000000000000000 ) ) ;
#12121 = CARTESIAN_POINT ( 'NONE',  ( -3.127054932750481964, -32.61873716947361856, 68.00000000000000000 ) ) ;
#12122 = ADVANCED_FACE ( 'NONE', ( #3684 ), #18881, .T. ) ;
#12123 = DIRECTION ( 'NONE',  ( 1.000000000000000000, 0.000000000000000000, 0.000000000000000000 ) ) ;
#12124 = CARTESIAN_POINT ( 'NONE',  ( 14.96174975910705918, -41.81054587065082728, 13.80000000000001315 ) ) ;
#12125 = LINE ( 'NONE', #12325, #21653 ) ;
#12126 = EDGE_CURVE ( 'NONE', #13130, #11811, #21748, .T. ) ;
#12127 = ORIENTED_EDGE ( 'NONE', *, *, #17349, .T. ) ;
#12128 = DIRECTION ( 'NONE',  ( 0.000000000000000000, 0.000000000000000000, -1.000000000000000000 ) ) ;
#12129 = CYLINDRICAL_SURFACE ( 'NONE', #16983, 0.04999999999999991257 ) ;
#12130 = FACE_OUTER_BOUND ( 'NONE', #17314, .T. ) ;
#12131 = ORIENTED_EDGE ( 'NONE', *, *, #1589, .T. ) ;
#12132 = EDGE_LOOP ( 'NONE', ( #1626, #358, #13700, #12601 ) ) ;
#12133 = ORIENTED_EDGE ( 'NONE', *, *, #15510, .T. ) ;
#12134 = CARTESIAN_POINT ( 'NONE',  ( 9.178906393579156386, 42.46645089659917716, 69.50000000000000000 ) ) ;
#12135 = DIRECTION ( 'NONE',  ( 1.000000000000000000, 0.000000000000000000, 0.000000000000000000 ) ) ;
#12136 = VECTOR ( 'NONE', #6595, 1000.000000000000000 ) ;
#12137 = AXIS2_PLACEMENT_3D ( 'NONE', #4987, #13910, #4872 ) ;
#12138 = DIRECTION ( 'NONE',  ( -1.000000000000000000, 0.000000000000000000, 0.000000000000000000 ) ) ;
#12139 = ORIENTED_EDGE ( 'NONE', *, *, #12106, .F. ) ;
#12140 = CYLINDRICAL_SURFACE ( 'NONE', #14676, 2.000000000000001776 ) ;
#12141 = ADVANCED_FACE ( 'NONE', ( #12376 ), #5814, .F. ) ;
#12142 = ORIENTED_EDGE ( 'NONE', *, *, #14328, .T. ) ;
#12143 = DIRECTION ( 'NONE',  ( 1.224646799147353207E-16, 0.000000000000000000, 1.000000000000000000 ) ) ;
#12144 = EDGE_CURVE ( 'NONE', #1591, #1902, #2438, .T. ) ;
#12145 = DIRECTION ( 'NONE',  ( -1.000000000000000000, 0.000000000000000000, 0.000000000000000000 ) ) ;
#12146 = CARTESIAN_POINT ( 'NONE',  ( -9.141460742840918030, -33.43424481021354921, 42.50000000000000000 ) ) ;
#12147 = EDGE_LOOP ( 'NONE', ( #2370, #15190, #15592, #14734 ) ) ;
#12148 = CARTESIAN_POINT ( 'NONE',  ( 23.29450335057348198, 3.413880037201885820, 13.50000000000000178 ) ) ;
#12149 = DIRECTION ( 'NONE',  ( 1.000000000000000000, 0.000000000000000000, 0.000000000000000000 ) ) ;
#12150 = AXIS2_PLACEMENT_3D ( 'NONE', #11079, #19468, #7405 ) ;
#12151 = CIRCLE ( 'NONE', #732, 0.2999999999999999334 ) ;
#12152 = FACE_OUTER_BOUND ( 'NONE', #1865, .T. ) ;
#12153 = PRODUCT_DEFINITION_SHAPE ( 'NONE', 'NONE',  #22168 ) ;
#12154 = PLANE ( 'NONE',  #2822 ) ;
#12155 = ORIENTED_EDGE ( 'NONE', *, *, #15632, .T. ) ;
#12156 = FILL_AREA_STYLE ('',( #12255 ) ) ;
#12157 = VERTEX_POINT ( 'NONE', #515 ) ;
#12158 = DIRECTION ( 'NONE',  ( 1.000000000000000000, 0.000000000000000000, 0.000000000000000000 ) ) ;
#12159 = EDGE_LOOP ( 'NONE', ( #16348, #19136, #18539, #12759 ) ) ;
#12160 = DIRECTION ( 'NONE',  ( -0.000000000000000000, -0.000000000000000000, -1.000000000000000000 ) ) ;
#12161 = ORIENTED_EDGE ( 'NONE', *, *, #16057, .T. ) ;
#12162 = PRODUCT_RELATED_PRODUCT_CATEGORY ( 'part', '', ( #20392 ) ) ;
#12163 = ORIENTED_EDGE ( 'NONE', *, *, #12800, .T. ) ;
#12164 = AXIS2_PLACEMENT_3D ( 'NONE', #21678, #21792, #18068 ) ;
#12165 = CIRCLE ( 'NONE', #15038, 0.2500000000000002220 ) ;
#12166 = VERTEX_POINT ( 'NONE', #3786 ) ;
#12167 = ORIENTED_EDGE ( 'NONE', *, *, #13334, .F. ) ;
#12168 = FACE_OUTER_BOUND ( 'NONE', #21080, .T. ) ;
#12169 = EDGE_CURVE ( 'NONE', #7877, #17755, #8514, .T. ) ;
#12170 = CARTESIAN_POINT ( 'NONE',  ( 34.39999999999998437, 84.70000000000001705, 80.00000000000000000 ) ) ;
#12171 = CYLINDRICAL_SURFACE ( 'NONE', #5323, 0.1000000000000028644 ) ;
#12172 = CIRCLE ( 'NONE', #21508, 0.05000000000000143219 ) ;
#12173 = DIRECTION ( 'NONE',  ( 0.000000000000000000, 0.000000000000000000, 1.000000000000000000 ) ) ;
#12174 = DIRECTION ( 'NONE',  ( -1.000000000000000000, 0.000000000000000000, 0.000000000000000000 ) ) ;
#12175 = AXIS2_PLACEMENT_3D ( 'NONE', #3994, #10810, #21116 ) ;
#12176 = CYLINDRICAL_SURFACE ( 'NONE', #18559, 4.351418481279137218 ) ;
#12177 = DIRECTION ( 'NONE',  ( -2.891205793294662845E-15, -0.000000000000000000, -1.000000000000000000 ) ) ;
#12178 = ORIENTED_EDGE ( 'NONE', *, *, #3556, .T. ) ;
#12179 = DIRECTION ( 'NONE',  ( -0.000000000000000000, -0.000000000000000000, 1.000000000000000000 ) ) ;
#12180 = CARTESIAN_POINT ( 'NONE',  ( -29.13662752439705272, 0.000000000000000000, -18.50000000000000000 ) ) ;
#12181 = AXIS2_PLACEMENT_3D ( 'NONE', #14905, #2952, #2607 ) ;
#12182 = ADVANCED_FACE ( 'NONE', ( #2318 ), #11354, .T. ) ;
#12183 = EDGE_LOOP ( 'NONE', ( #4751, #6951, #15017, #10330 ) ) ;
#12184 = ORIENTED_EDGE ( 'NONE', *, *, #4636, .F. ) ;
#12185 = DIRECTION ( 'NONE',  ( 0.000000000000000000, 0.000000000000000000, 1.000000000000000000 ) ) ;
#12186 = SHAPE_DEFINITION_REPRESENTATION ( #10395, #10840 ) ;
#12187 = AXIS2_PLACEMENT_3D ( 'NONE', #13235, #19844, #20079 ) ;
#12188 = VERTEX_POINT ( 'NONE', #12264 ) ;
#12189 = CIRCLE ( 'NONE', #13982, 0.1000000000000028644 ) ;
#12190 = ADVANCED_FACE ( 'NONE', ( #15743 ), #8170, .T. ) ;
#12191 = CARTESIAN_POINT ( 'NONE',  ( 23.02398829872513986, -3.418849134688107139, 13.52821124852847134 ) ) ;
#12192 = VERTEX_POINT ( 'NONE', #17426 ) ;
#12193 = EDGE_LOOP ( 'NONE', ( #18636, #10781, #14620, #15843, #9388 ) ) ;
#12194 = CARTESIAN_POINT ( 'NONE',  ( 9.178906393579156386, 42.46645089659917716, 69.50000000000000000 ) ) ;
#12195 = FACE_OUTER_BOUND ( 'NONE', #20617, .T. ) ;
#12196 = CARTESIAN_POINT ( 'NONE',  ( -6.728906393579160650, 43.00645089659919762, 70.88527860057354246 ) ) ;
#12197 = AXIS2_PLACEMENT_3D ( 'NONE', #10710, #17526, #2195 ) ;
#12198 = DIRECTION ( 'NONE',  ( -0.000000000000000000, -0.000000000000000000, -1.000000000000000000 ) ) ;
#12199 = AXIS2_PLACEMENT_3D ( 'NONE', #14771, #6289, #4610 ) ;
#12200 = LINE ( 'NONE', #8978, #10113 ) ;
#12201 = VECTOR ( 'NONE', #2801, 1000.000000000000000 ) ;
#12202 = AXIS2_PLACEMENT_3D ( 'NONE', #19123, #8510, #15327 ) ;
#12203 = DIRECTION ( 'NONE',  ( 0.000000000000000000, -0.000000000000000000, -1.000000000000000000 ) ) ;
#12204 = CARTESIAN_POINT ( 'NONE',  ( 23.04273156199908357, -2.261510999192740901, 13.19999999999999929 ) ) ;
#12205 = CARTESIAN_POINT ( 'NONE',  ( -30.19999999999999574, 70.29999999999999716, 1.500000000000000222 ) ) ;
#12206 = EDGE_CURVE ( 'NONE', #6508, #18412, #2101, .T. ) ;
#12207 = DIRECTION ( 'NONE',  ( 0.000000000000000000, 0.000000000000000000, 1.000000000000000000 ) ) ;
#12208 = EDGE_LOOP ( 'NONE', ( #9732, #1030, #19491, #9512, #9744, #12209 ) ) ;
#12209 = ORIENTED_EDGE ( 'NONE', *, *, #345, .F. ) ;
#12210 = CARTESIAN_POINT ( 'NONE',  ( -1.774728116533986766, 42.36054587065083155, 45.66679706732590205 ) ) ;
#12211 = LINE ( 'NONE', #19283, #8488 ) ;
#12212 = VERTEX_POINT ( 'NONE', #15954 ) ;
#12213 = EDGE_CURVE ( 'NONE', #2230, #20083, #8940, .T. ) ;
#12214 = VECTOR ( 'NONE', #19455, 1000.000000000000000 ) ;
#12215 = EDGE_CURVE ( 'NONE', #12408, #7436, #7370, .T. ) ;
#12216 = CIRCLE ( 'NONE', #14012, 0.2999999999999999334 ) ;
#12217 = EDGE_CURVE ( 'NONE', #21878, #9228, #16070, .T. ) ;
#12218 = EDGE_CURVE ( 'NONE', #483, #17330, #16412, .T. ) ;
#12219 = FACE_OUTER_BOUND ( 'NONE', #20089, .T. ) ;
#12220 = CARTESIAN_POINT ( 'NONE',  ( 29.17540678000427690, 0.000000000000000000, 7.799999999999999822 ) ) ;
#12221 = ORIENTED_EDGE ( 'NONE', *, *, #17047, .F. ) ;
#12222 = DIRECTION ( 'NONE',  ( 0.000000000000000000, 0.000000000000000000, -1.000000000000000000 ) ) ;
#12223 = TOROIDAL_SURFACE ( 'NONE', #1523, 0.05000000000000000278, 0.05000000000000000278 ) ;
#12224 = CARTESIAN_POINT ( 'NONE',  ( -21.92816239687475743, 42.46645089659918426, 68.50000000000000000 ) ) ;
#12225 = DIRECTION ( 'NONE',  ( 1.000000000000000000, 0.000000000000000000, 6.123233995736764803E-17 ) ) ;
#12226 = DIRECTION ( 'NONE',  ( -1.000000000000000000, 0.000000000000000000, 0.000000000000000000 ) ) ;
#12227 = DIRECTION ( 'NONE',  ( 1.000000000000000000, 0.000000000000000000, 0.000000000000000000 ) ) ;
#12228 = DIRECTION ( 'NONE',  ( 1.000000000000000000, -0.000000000000000000, -0.000000000000000000 ) ) ;
#12229 = EDGE_CURVE ( 'NONE', #10879, #7401, #266, .T. ) ;
#12230 = EDGE_LOOP ( 'NONE', ( #19281, #3789, #14317, #19846, #21498, #11907 ) ) ;
#12231 = CARTESIAN_POINT ( 'NONE',  ( -3.627054932750481964, 32.93424481021354921, 13.50000000000000000 ) ) ;
#12232 = DIRECTION ( 'NONE',  ( 0.000000000000000000, 0.000000000000000000, 1.000000000000000000 ) ) ;
#12233 = PLANE ( 'NONE',  #6704 ) ;
#12234 = ORIENTED_EDGE ( 'NONE', *, *, #19816, .T. ) ;
#12235 = ORIENTED_EDGE ( 'NONE', *, *, #11145, .T. ) ;
#12236 = VERTEX_POINT ( 'NONE', #2545 ) ;
#12237 = CARTESIAN_POINT ( 'NONE',  ( 23.02398829872513986, 7.027230193580998154E-15, 42.50000000000000000 ) ) ;
#12238 = CARTESIAN_POINT ( 'NONE',  ( 0.000000000000000000, 43.31054587065082728, 8.000000000000000000 ) ) ;
#12239 = FACE_OUTER_BOUND ( 'NONE', #20115, .T. ) ;
#12240 = EDGE_CURVE ( 'NONE', #11281, #17419, #4558, .T. ) ;
#12241 = VERTEX_POINT ( 'NONE', #13163 ) ;
#12242 = DIRECTION ( 'NONE',  ( -0.000000000000000000, -0.000000000000000000, -1.000000000000000000 ) ) ;
#12243 = EDGE_CURVE ( 'NONE', #1577, #20269, #20295, .T. ) ;
#12244 = ORIENTED_EDGE ( 'NONE', *, *, #10892, .T. ) ;
#12245 = DIRECTION ( 'NONE',  ( 0.9729678061520314891, 0.2309407893632107189, 0.000000000000000000 ) ) ;
#12246 = LINE ( 'NONE', #18763, #5679 ) ;
#12247 = CARTESIAN_POINT ( 'NONE',  ( -29.17540678000427690, -6.499884319688664647, 7.500000000000000000 ) ) ;
#12248 = CARTESIAN_POINT ( 'NONE',  ( -32.47706987357030073, 83.66206381164208494, 68.50000000000000000 ) ) ;
#12249 = ORIENTED_EDGE ( 'NONE', *, *, #623, .F. ) ;
#12250 = CARTESIAN_POINT ( 'NONE',  ( 29.13662752439705272, 0.000000000000000000, 0.3000000000000016542 ) ) ;
#12251 = DIRECTION ( 'NONE',  ( -0.000000000000000000, 0.000000000000000000, 1.000000000000000000 ) ) ;
#12252 = CARTESIAN_POINT ( 'NONE',  ( 3.127054932750481964, -32.93424481021354921, 68.00000000000000000 ) ) ;
#12253 = CARTESIAN_POINT ( 'NONE',  ( -25.37540678000429395, -39.04634676501046187, 13.79999999999999893 ) ) ;
#12254 = ORIENTED_EDGE ( 'NONE', *, *, #13327, .T. ) ;
#12255 = FILL_AREA_STYLE_COLOUR ( '', #8771 ) ;
#12256 = ORIENTED_EDGE ( 'NONE', *, *, #3942, .F. ) ;
#12257 = CYLINDRICAL_SURFACE ( 'NONE', #2321, 0.5000000000000004441 ) ;
#12258 = CARTESIAN_POINT ( 'NONE',  ( -21.91689697940243775, 45.66657467514198743, 68.25000000000000000 ) ) ;
#12259 =( BOUNDED_SURFACE ( )  B_SPLINE_SURFACE ( 3, 2, ( 
 ( #11820, #5131, #10593 ),
 ( #1964, #16972, #19101 ),
 ( #294, #17097, #18769 ),
 ( #8811, #12041, #7033 ),
 ( #1871, #13827, #18890 ),
 ( #18658, #10276, #3442 ),
 ( #8605, #20791, #3770 ),
 ( #8485, #20685, #1215 ),
 ( #5243, #15302, #15413 ),
 ( #87, #13716, #3565 ),
 ( #8066, #14871, #12148 ),
 ( #10389, #179, #3670 ) ),
 .UNSPECIFIED., .F., .F., .T. ) 
 B_SPLINE_SURFACE_WITH_KNOTS ( ( 4, 2, 2, 2, 2, 4 ),
 ( 3, 3 ),
 ( 0.0007953085288493483155, 0.0009951922240469498245, 0.001195075919244551225, 0.001594843309639754243, 0.001994610700034957045, 0.002394378090430160280 ),
 ( 0.000000000000000000, 1.000000000000000000 ),
 .UNSPECIFIED. ) 
 GEOMETRIC_REPRESENTATION_ITEM ( )  RATIONAL_B_SPLINE_SURFACE ( (
 ( 1.000000000000000000, 0.9842566880020464648, 1.000000000000000000),
 ( 1.000000000000000000, 0.9842682545141110406, 1.000000000000000000),
 ( 1.000000000000000000, 0.9790935905989446297, 1.000000000000000000),
 ( 1.000000000000000000, 0.9652215946044104822, 1.000000000000000000),
 ( 1.000000000000000000, 0.9566241109334278070, 1.000000000000000000),
 ( 1.000000000000000000, 0.9283687200450853050, 1.000000000000000000),
 ( 1.000000000000000000, 0.9065874062052554638, 1.000000000000000000),
 ( 1.000000000000000000, 0.8577429740253610380, 1.000000000000000000),
 ( 1.000000000000000000, 0.8312249658974324440, 1.000000000000000000),
 ( 1.000000000000000000, 0.7732701221512614520, 1.000000000000000000),
 ( 1.000000000000000000, 0.7418345472258666140, 1.000000000000000000),
 ( 1.000000000000000000, 0.7071067811865475727, 1.000000000000000000) ) ) 
 REPRESENTATION_ITEM ( '' )  SURFACE ( )  );
#12260 = VERTEX_POINT ( 'NONE', #8032 ) ;
#12261 = EDGE_LOOP ( 'NONE', ( #6147, #12119, #7952, #3370 ) ) ;
#12262 = DIRECTION ( 'NONE',  ( 0.000000000000000000, -1.000000000000000000, 0.000000000000000000 ) ) ;
#12263 = ADVANCED_FACE ( 'NONE', ( #9472 ), #13035, .F. ) ;
#12264 = CARTESIAN_POINT ( 'NONE',  ( 17.95292532278785913, -50.11873716947361856, 13.99999999999999822 ) ) ;
#12265 = ORIENTED_EDGE ( 'NONE', *, *, #12540, .T. ) ;
#12266 = CIRCLE ( 'NONE', #2634, 0.2500000000000002220 ) ;
#12267 = ORIENTED_EDGE ( 'NONE', *, *, #27, .T. ) ;
#12268 = ADVANCED_FACE ( 'NONE', ( #11377 ), #17866, .T. ) ;
#12269 = ORIENTED_EDGE ( 'NONE', *, *, #7943, .F. ) ;
#12270 = DIRECTION ( 'NONE',  ( 2.107255972849994642E-16, -0.000000000000000000, 1.000000000000000000 ) ) ;
#12271 = AXIS2_PLACEMENT_3D ( 'NONE', #15439, #5051, #20052 ) ;
#12272 = CARTESIAN_POINT ( 'NONE',  ( -1.724728116533986721, 43.26054587065083012, 41.66679706732590915 ) ) ;
#12273 = AXIS2_PLACEMENT_3D ( 'NONE', #2530, #16161, #21340 ) ;
#12274 = DIRECTION ( 'NONE',  ( 1.000000000000000000, 0.000000000000000000, -2.388292521039847891E-16 ) ) ;
#12275 = CARTESIAN_POINT ( 'NONE',  ( -1.824728116533986810, 43.31054587065082728, 51.70876104995653577 ) ) ;
#12276 = UNCERTAINTY_MEASURE_WITH_UNIT (LENGTH_MEASURE( 1.000000000000000082E-05 ), #2697, 'distance_accuracy_value', 'NONE');
#12277 = EDGE_LOOP ( 'NONE', ( #8791, #14601, #3982, #4555 ) ) ;
#12278 = CARTESIAN_POINT ( 'NONE',  ( 29.44686415200675711, 2.575389668538635046, 0.1239436336148718037 ) ) ;
#12279 = PLANE ( 'NONE',  #6544 ) ;
#12280 = VERTEX_POINT ( 'NONE', #1083 ) ;
#12281 = EDGE_CURVE ( 'NONE', #627, #13557, #6737, .T. ) ;
#12282 = PLANE ( 'NONE',  #20994 ) ;
#12283 = ORIENTED_EDGE ( 'NONE', *, *, #6338, .T. ) ;
#12284 = EDGE_CURVE ( 'NONE', #13976, #9183, #1183, .T. ) ;
#12285 = ORIENTED_EDGE ( 'NONE', *, *, #5455, .F. ) ;
#12286 = ORIENTED_EDGE ( 'NONE', *, *, #18225, .F. ) ;
#12287 = CARTESIAN_POINT ( 'NONE',  ( -29.17540678000427690, 63.74634676501045050, 7.799999999999999822 ) ) ;
#12288 = DIRECTION ( 'NONE',  ( 0.000000000000000000, 0.000000000000000000, -1.000000000000000000 ) ) ;
#12289 = VERTEX_POINT ( 'NONE', #16281 ) ;
#12290 = CARTESIAN_POINT ( 'NONE',  ( -17.95292532278785913, -50.11873716947361856, 68.00000000000000000 ) ) ;
#12291 = ORIENTED_EDGE ( 'NONE', *, *, #4734, .F. ) ;
#12292 = ORIENTED_EDGE ( 'NONE', *, *, #13614, .F. ) ;
#12293 = DIRECTION ( 'NONE',  ( -1.224646799147353207E-16, -0.000000000000000000, -1.000000000000000000 ) ) ;
#12294 = CARTESIAN_POINT ( 'NONE',  ( 27.37540678000427974, -10.94079601157914716, 13.79999999999999893 ) ) ;
#12295 =( NAMED_UNIT ( * ) PLANE_ANGLE_UNIT ( ) SI_UNIT ( $, .RADIAN. ) );
#12296 = CARTESIAN_POINT ( 'NONE',  ( -1.774728116533986766, 42.36054587065083155, 49.66679706732590915 ) ) ;
#12297 = EDGE_CURVE ( 'NONE', #20541, #19733, #4598, .T. ) ;
#12298 = CIRCLE ( 'NONE', #13388, 0.2999999999999999334 ) ;
#12299 = CIRCLE ( 'NONE', #2672, 0.2999999999999999334 ) ;
#12300 = CARTESIAN_POINT ( 'NONE',  ( -23.02398829872514341, 2.624711895713190302, 13.63074282194510189 ) ) ;
#12301 = DIRECTION ( 'NONE',  ( -0.000000000000000000, -1.000000000000000000, -0.000000000000000000 ) ) ;
#12302 = DIRECTION ( 'NONE',  ( 0.000000000000000000, 0.000000000000000000, 1.000000000000000000 ) ) ;
#12303 = DIRECTION ( 'NONE',  ( -1.000000000000000000, 0.000000000000000000, 0.000000000000000000 ) ) ;
#12304 = ADVANCED_FACE ( 'NONE', ( #2888 ), #9715, .T. ) ;
#12305 = DIRECTION ( 'NONE',  ( -1.000000000000000000, 0.000000000000000000, 0.000000000000000000 ) ) ;
#12306 = ORIENTED_EDGE ( 'NONE', *, *, #14275, .T. ) ;
#12307 = ORIENTED_EDGE ( 'NONE', *, *, #2588, .T. ) ;
#12308 = DIRECTION ( 'NONE',  ( -1.000000000000000000, 0.000000000000000000, 0.000000000000000000 ) ) ;
#12309 =( NAMED_UNIT ( * ) PLANE_ANGLE_UNIT ( ) SI_UNIT ( $, .RADIAN. ) );
#12310 = VERTEX_POINT ( 'NONE', #7695 ) ;
#12311 = TOROIDAL_SURFACE ( 'NONE', #14471, 4.051418481279137396, 0.2999999999999999889 ) ;
#12312 = FACE_OUTER_BOUND ( 'NONE', #5442, .T. ) ;
#12313 = CIRCLE ( 'NONE', #888, 0.2500000000000002220 ) ;
#12314 = ORIENTED_EDGE ( 'NONE', *, *, #20474, .F. ) ;
#12315 = EDGE_CURVE ( 'NONE', #11313, #11863, #19550, .T. ) ;
#12316 = FACE_OUTER_BOUND ( 'NONE', #20138, .T. ) ;
#12317 = DIRECTION ( 'NONE',  ( 0.000000000000000000, -0.000000000000000000, -1.000000000000000000 ) ) ;
#12318 = CIRCLE ( 'NONE', #6652, 0.2999999999999999334 ) ;
#12319 = ORIENTED_EDGE ( 'NONE', *, *, #16224, .T. ) ;
#12320 = FACE_BOUND ( 'NONE', #1472, .T. ) ;
#12321 = DIRECTION ( 'NONE',  ( 0.000000000000000000, 1.000000000000000000, -0.000000000000000000 ) ) ;
#12322 = LINE ( 'NONE', #9325, #19710 ) ;
#12323 = LINE ( 'NONE', #10364, #18565 ) ;
#12324 = DIRECTION ( 'NONE',  ( 0.000000000000000000, 1.000000000000000000, 0.000000000000000000 ) ) ;
#12325 = CARTESIAN_POINT ( 'NONE',  ( -29.17540678000427690, 0.000000000000000000, 7.500000000000000000 ) ) ;
#12326 = AXIS2_PLACEMENT_3D ( 'NONE', #4149, #7407, #5515 ) ;
#12327 = MECHANICAL_DESIGN_GEOMETRIC_PRESENTATION_REPRESENTATION (  '', ( #522 ), #2336 ) ;
#12328 = VECTOR ( 'NONE', #10816, 1000.000000000000000 ) ;
#12329 = ADVANCED_FACE ( 'NONE', ( #14618 ), #851, .T. ) ;
#12330 = VERTEX_POINT ( 'NONE', #2765 ) ;
#12331 = DIRECTION ( 'NONE',  ( 0.000000000000000000, 0.000000000000000000, -1.000000000000000000 ) ) ;
#12332 = DIRECTION ( 'NONE',  ( -1.000000000000000000, 0.000000000000000000, 0.000000000000000000 ) ) ;
#12333 = EDGE_CURVE ( 'NONE', #9267, #13403, #21044, .T. ) ;
#12334 = DIRECTION ( 'NONE',  ( -0.000000000000000000, 1.000000000000000000, -0.000000000000000000 ) ) ;
#12335 = ORIENTED_EDGE ( 'NONE', *, *, #9994, .F. ) ;
#12336 = ORIENTED_EDGE ( 'NONE', *, *, #3779, .F. ) ;
#12337 = ORIENTED_EDGE ( 'NONE', *, *, #15931, .T. ) ;
#12338 = CARTESIAN_POINT ( 'NONE',  ( -29.09616841400578124, -6.500357067309672665, 7.499999999999999112 ) ) ;
#12339 = CARTESIAN_POINT ( 'NONE',  ( -15.21174975910705207, 41.81054587065082728, 68.25000000000000000 ) ) ;
#12340 = CARTESIAN_POINT ( 'NONE',  ( 25.37540678000429395, -39.04634676501046187, 13.79999999999999893 ) ) ;
#12341 = EDGE_LOOP ( 'NONE', ( #15178, #9368, #13480, #16542, #7186, #7278, #2719, #966 ) ) ;
#12342 = AXIS2_PLACEMENT_3D ( 'NONE', #6827, #22029, #13510 ) ;
#12343 = AXIS2_PLACEMENT_3D ( 'NONE', #13580, #20527, #3067 ) ;
#12344 = DIRECTION ( 'NONE',  ( 0.000000000000000000, 0.000000000000000000, 1.000000000000000000 ) ) ;
#12345 = VECTOR ( 'NONE', #5300, 1000.000000000000000 ) ;
#12346 = ORIENTED_EDGE ( 'NONE', *, *, #18621, .F. ) ;
#12347 = CARTESIAN_POINT ( 'NONE',  ( 29.69597781366221767, 26.24124249474150972, 68.75000000000000000 ) ) ;
#12348 = CIRCLE ( 'NONE', #20238, 4.700000000000002842 ) ;
#12349 = EDGE_CURVE ( 'NONE', #10209, #9996, #15313, .T. ) ;
#12350 = ORIENTED_EDGE ( 'NONE', *, *, #4213, .T. ) ;
#12351 = CARTESIAN_POINT ( 'NONE',  ( 25.37540678000429395, -38.74634676501045760, 42.50000000000000000 ) ) ;
#12352 = CARTESIAN_POINT ( 'NONE',  ( -25.37540678000426908, 36.74634676501047181, 13.50000000000000000 ) ) ;
#12353 = FACE_OUTER_BOUND ( 'NONE', #20499, .T. ) ;
#12354 = DIRECTION ( 'NONE',  ( 1.000000000000000000, 0.000000000000000000, 0.000000000000000000 ) ) ;
#12355 = ORIENTED_EDGE ( 'NONE', *, *, #9770, .F. ) ;
#12356 = CARTESIAN_POINT ( 'NONE',  ( 1.724728116533979616, 43.26054587065083012, 27.75876104995653648 ) ) ;
#12357 = DIRECTION ( 'NONE',  ( 0.000000000000000000, 0.000000000000000000, 1.000000000000000000 ) ) ;
#12358 = DIRECTION ( 'NONE',  ( 0.000000000000000000, 0.000000000000000000, 1.000000000000000000 ) ) ;
#12359 = DIRECTION ( 'NONE',  ( 0.000000000000000000, 1.000000000000000000, 0.000000000000000000 ) ) ;
#12360 = ORIENTED_EDGE ( 'NONE', *, *, #20692, .T. ) ;
#12361 = VECTOR ( 'NONE', #18053, 1000.000000000000000 ) ;
#12362 = VECTOR ( 'NONE', #12007, 1000.000000000000000 ) ;
#12363 = AXIS2_PLACEMENT_3D ( 'NONE', #15275, #22007, #18634 ) ;
#12364 = CARTESIAN_POINT ( 'NONE',  ( -1.724728116533986721, 42.36054587065083155, 39.80876104995653719 ) ) ;
#12365 = AXIS2_PLACEMENT_3D ( 'NONE', #16778, #8390, #1448 ) ;
#12366 = ADVANCED_FACE ( 'NONE', ( #2649 ), #304, .F. ) ;
#12367 = ORIENTED_EDGE ( 'NONE', *, *, #21569, .T. ) ;
#12368 = CARTESIAN_POINT ( 'NONE',  ( 17.95292532278785913, 50.11873716947361856, 13.99999999999999822 ) ) ;
#12369 = ADVANCED_FACE ( 'NONE', ( #9881 ), #14226, .T. ) ;
#12370 = DIRECTION ( 'NONE',  ( 0.000000000000000000, 0.000000000000000000, -1.000000000000000000 ) ) ;
#12371 = EDGE_LOOP ( 'NONE', ( #4164, #8036, #2007, #5343 ) ) ;
#12372 = CIRCLE ( 'NONE', #4163, 3.500000000000003109 ) ;
#12373 = EDGE_LOOP ( 'NONE', ( #9738, #7489, #19164, #2835 ) ) ;
#12375 = EDGE_CURVE ( 'NONE', #8611, #16245, #15234, .T. ) ;
#12374 = FACE_OUTER_BOUND ( 'NONE', #6416, .T. ) ;
#12376 = FACE_OUTER_BOUND ( 'NONE', #17647, .T. ) ;
#12377 = ORIENTED_EDGE ( 'NONE', *, *, #13546, .T. ) ;
#12378 = TOROIDAL_SURFACE ( 'NONE', #15956, 2.274596669241483848, 0.2999999999999999889 ) ;
#12379 = ORIENTED_EDGE ( 'NONE', *, *, #280, .T. ) ;
#12380 = VECTOR ( 'NONE', #4707, 1000.000000000000000 ) ;
#12381 = AXIS2_PLACEMENT_3D ( 'NONE', #10472, #15815, #13698 ) ;
#12382 = TOROIDAL_SURFACE ( 'NONE', #19541, 0.5000000000000000000, 0.2500000000000000000 ) ;
#12383 = EDGE_CURVE ( 'NONE', #10729, #17715, #130, .T. ) ;
#12384 = DIRECTION ( 'NONE',  ( -0.000000000000000000, 0.000000000000000000, 1.000000000000000000 ) ) ;
#12385 = DIRECTION ( 'NONE',  ( 1.000000000000000000, 0.000000000000000000, 0.000000000000000000 ) ) ;
#12386 = AXIS2_PLACEMENT_3D ( 'NONE', #3845, #6894, #14106 ) ;
#12387 = AXIS2_PLACEMENT_3D ( 'NONE', #15063, #4439, #18077 ) ;
#12388 = DIRECTION ( 'NONE',  ( -0.000000000000000000, -1.000000000000000000, -0.000000000000000000 ) ) ;
#12389 = CARTESIAN_POINT ( 'NONE',  ( 1.774728116533979438, 42.36054587065083155, 51.80876104995653719 ) ) ;
#12390 = EDGE_CURVE ( 'NONE', #17937, #21191, #9952, .T. ) ;
#12391 = EDGE_LOOP ( 'NONE', ( #20331, #3703, #10707, #18774 ) ) ;
#12392 =( BOUNDED_CURVE ( )  B_SPLINE_CURVE ( 3, ( #17099, #22156, #21923, #8267 ),
 .UNSPECIFIED., .F., .T. ) 
 B_SPLINE_CURVE_WITH_KNOTS ( ( 4, 4 ),
 ( 4.712388980384689674, 6.283185307179586232 ),
 .UNSPECIFIED. ) 
 CURVE ( )  GEOMETRIC_REPRESENTATION_ITEM ( )  RATIONAL_B_SPLINE_CURVE ( ( 1.000000000000000000, 0.8047378541243649375, 0.8047378541243649375, 1.000000000000000000 ) ) 
 REPRESENTATION_ITEM ( '' )  );
#12393 = CARTESIAN_POINT ( 'NONE',  ( 1.724728116533979838, 43.31054587065082728, 29.66679706732590560 ) ) ;
#12394 = FACE_OUTER_BOUND ( 'NONE', #19584, .T. ) ;
#12395 = VECTOR ( 'NONE', #13278, 1000.000000000000000 ) ;
#12396 = AXIS2_PLACEMENT_3D ( 'NONE', #5266, #18679, #13534 ) ;
#12397 = CIRCLE ( 'NONE', #12055, 0.05000000000000143219 ) ;
#12398 = EDGE_CURVE ( 'NONE', #12330, #8378, #11725, .T. ) ;
#12399 = ORIENTED_EDGE ( 'NONE', *, *, #11145, .F. ) ;
#12400 = DIRECTION ( 'NONE',  ( -0.000000000000000000, -0.000000000000000000, -1.000000000000000000 ) ) ;
#12401 = ORIENTED_EDGE ( 'NONE', *, *, #10560, .F. ) ;
#12402 = AXIS2_PLACEMENT_3D ( 'NONE', #6331, #11458, #19519 ) ;
#12403 = ORIENTED_EDGE ( 'NONE', *, *, #21199, .T. ) ;
#12404 = ORIENTED_EDGE ( 'NONE', *, *, #4968, .F. ) ;
#12405 = CARTESIAN_POINT ( 'NONE',  ( 30.67540678000428045, -63.74634676501045050, 3.500000000000000000 ) ) ;
#12406 = TOROIDAL_SURFACE ( 'NONE', #17783, 3.800000000000002931, 0.2999999999999999889 ) ;
#12407 = PRODUCT_CONTEXT ( 'NONE', #6897, 'mechanical' ) ;
#12408 = VERTEX_POINT ( 'NONE', #13668 ) ;
#12409 = EDGE_LOOP ( 'NONE', ( #7959, #18561, #15025, #20171 ) ) ;
#12410 = CARTESIAN_POINT ( 'NONE',  ( 23.29441641503727567, -3.413540866333718338, 13.50000000000000000 ) ) ;
#12411 = VERTEX_POINT ( 'NONE', #15024 ) ;
#12412 = AXIS2_PLACEMENT_3D ( 'NONE', #4023, #2218, #9051 ) ;
#12413 = VECTOR ( 'NONE', #5892, 1000.000000000000000 ) ;
#12414 = AXIS2_PLACEMENT_3D ( 'NONE', #18206, #14832, #4441 ) ;
#12415 = EDGE_LOOP ( 'NONE', ( #1761, #6684, #13053, #10776 ) ) ;
#12416 = EDGE_CURVE ( 'NONE', #8409, #4651, #20073, .T. ) ;
#12417 = DIRECTION ( 'NONE',  ( 0.000000000000000000, 0.000000000000000000, 1.000000000000000000 ) ) ;
#12418 = CARTESIAN_POINT ( 'NONE',  ( 0.000000000000000000, -68.74634676501045760, 3.799999999999999822 ) ) ;
#12419 = EDGE_CURVE ( 'NONE', #16692, #630, #18826, .T. ) ;
#12420 = AXIS2_PLACEMENT_3D ( 'NONE', #12389, #14183, #21039 ) ;
#12421 = EDGE_CURVE ( 'NONE', #15670, #10812, #6980, .T. ) ;
#12422 = AXIS2_PLACEMENT_3D ( 'NONE', #16677, #21961, #18361 ) ;
#12423 = DIRECTION ( 'NONE',  ( 0.000000000000000000, -1.000000000000000000, 0.000000000000000000 ) ) ;
#12424 = CARTESIAN_POINT ( 'NONE',  ( -23.13130088652691541, 2.712279394122547593, 13.41537141447312109 ) ) ;
#12425 = DIRECTION ( 'NONE',  ( -1.000000000000000000, 0.000000000000000000, 0.000000000000000000 ) ) ;
#12426 = CARTESIAN_POINT ( 'NONE',  ( 23.04392555272741205, -2.268071869891188364, 13.22877247997975481 ) ) ;
#12427 = LINE ( 'NONE', #15790, #13274 ) ;
#12428 = CIRCLE ( 'NONE', #5273, 0.2999999999999999334 ) ;
#12429 = CIRCLE ( 'NONE', #8549, 1.974596669241483804 ) ;
#12430 = ORIENTED_EDGE ( 'NONE', *, *, #3503, .T. ) ;
#12431 = ORIENTED_EDGE ( 'NONE', *, *, #12984, .F. ) ;
#12432 = CARTESIAN_POINT ( 'NONE',  ( 1.724728116533979616, 43.31054587065082728, 47.80876104995653719 ) ) ;
#12433 = VERTEX_POINT ( 'NONE', #6765 ) ;
#12434 = CIRCLE ( 'NONE', #2810, 0.6999999999999992895 ) ;
#12435 = ORIENTED_EDGE ( 'NONE', *, *, #9838, .T. ) ;
#12436 = B_SPLINE_CURVE_WITH_KNOTS ( 'NONE', 3,
 ( #14802, #6217, #17943, #21320, #7900, #2617, #11223, #6325 ),
 .UNSPECIFIED., .F., .F.,
 ( 4, 2, 2, 4 ),
 ( 0.000000000000000000, 0.0002393859945378754744, 0.0003590789918068118427, 0.0004787719890757481840 ),
 .UNSPECIFIED. ) ;
#12437 = VECTOR ( 'NONE', #874, 1000.000000000000000 ) ;
#12438 = ORIENTED_EDGE ( 'NONE', *, *, #7063, .T. ) ;
#12439 = AXIS2_PLACEMENT_3D ( 'NONE', #5934, #2566, #16303 ) ;
#12440 = ADVANCED_FACE ( 'NONE', ( #10213 ), #6645, .F. ) ;
#12441 = DIRECTION ( 'NONE',  ( 1.224646799147353207E-16, 0.000000000000000000, 1.000000000000000000 ) ) ;
#12442 = ADVANCED_FACE ( 'NONE', ( #6548 ), #11648, .F. ) ;
#12443 = CIRCLE ( 'NONE', #5709, 1.000000000000000888 ) ;
#12444 = LINE ( 'NONE', #1932, #5950 ) ;
#12445 = ORIENTED_EDGE ( 'NONE', *, *, #6674, .F. ) ;
#12446 = CARTESIAN_POINT ( 'NONE',  ( -3.127054932750481964, 32.93424481021354921, 68.00000000000000000 ) ) ;
#12447 = DIRECTION ( 'NONE',  ( 0.000000000000000000, 0.000000000000000000, 1.000000000000000000 ) ) ;
#12448 = LINE ( 'NONE', #5542, #20071 ) ;
#12449 = DIRECTION ( 'NONE',  ( 0.000000000000000000, 0.000000000000000000, 1.000000000000000000 ) ) ;
#12450 = CYLINDRICAL_SURFACE ( 'NONE', #10075, 0.05000000000000143219 ) ;
#12451 = LINE ( 'NONE', #20868, #13758 ) ;
#12452 = CIRCLE ( 'NONE', #7496, 0.1000000000000028644 ) ;
#12453 = CARTESIAN_POINT ( 'NONE',  ( 1.774728116533979883, 43.26054587065083012, 37.66679706732590915 ) ) ;
#12454 = PLANE ( 'NONE',  #19488 ) ;
#12455 = CARTESIAN_POINT ( 'NONE',  ( 1.774728116533979438, 43.31054587065082728, 47.80876104995653719 ) ) ;
#12456 = ORIENTED_EDGE ( 'NONE', *, *, #20977, .F. ) ;
#12457 = VERTEX_POINT ( 'NONE', #18484 ) ;
#12458 = DIRECTION ( 'NONE',  ( -0.000000000000000000, -0.000000000000000000, -1.000000000000000000 ) ) ;
#12459 = CARTESIAN_POINT ( 'NONE',  ( -1.724728116533986721, 43.31054587065082728, 29.66679706732590560 ) ) ;
#12460 = VERTEX_POINT ( 'NONE', #11544 ) ;
#12461 = CARTESIAN_POINT ( 'NONE',  ( -1.824728116533986810, 42.36054587065083155, 37.76679706732590347 ) ) ;
#12462 = VECTOR ( 'NONE', #4478, 1000.000000000000000 ) ;
#12463 = VERTEX_POINT ( 'NONE', #20170 ) ;
#12464 = CYLINDRICAL_SURFACE ( 'NONE', #12175, 0.05000000000000143219 ) ;
#12465 = CARTESIAN_POINT ( 'NONE',  ( -25.37540678000429395, -38.74634676501045760, 42.50000000000000000 ) ) ;
#12466 = EDGE_CURVE ( 'NONE', #5063, #17549, #4839, .T. ) ;
#12467 = EDGE_LOOP ( 'NONE', ( #6949, #14434, #8667, #12178 ) ) ;
#12468 = DIRECTION ( 'NONE',  ( -0.000000000000000000, 0.000000000000000000, 1.000000000000000000 ) ) ;
#12469 = EDGE_CURVE ( 'NONE', #3984, #13615, #2804, .T. ) ;
#12470 = CARTESIAN_POINT ( 'NONE',  ( -1.724728116533986721, 43.26054587065083012, 33.76679706732591058 ) ) ;
#12471 = DIRECTION ( 'NONE',  ( 0.000000000000000000, 0.000000000000000000, 1.000000000000000000 ) ) ;
#12472 = CARTESIAN_POINT ( 'NONE',  ( 31.50000000000002132, -72.00000000000001421, 3.200000000000000178 ) ) ;
#12473 = ORIENTED_EDGE ( 'NONE', *, *, #18649, .T. ) ;
#12474 = CARTESIAN_POINT ( 'NONE',  ( 32.50000000000002132, 71.00000000000001421, 1.800000000000000044 ) ) ;
#12475 = CARTESIAN_POINT ( 'NONE',  ( -29.69597781366221767, 56.94165929845684815, 68.75000000000000000 ) ) ;
#12476 = CYLINDRICAL_SURFACE ( 'NONE', #20525, 1.000000000000000888 ) ;
#12477 = CARTESIAN_POINT ( 'NONE',  ( -23.14059574490498505, -2.755557770589328381, 13.42404417222473612 ) ) ;
#12478 = ORIENTED_EDGE ( 'NONE', *, *, #18176, .F. ) ;
#12480 = CIRCLE ( 'NONE', #2856, 0.1000000000000028644 ) ;
#12479 = DIRECTION ( 'NONE',  ( 0.000000000000000000, 0.000000000000000000, 1.000000000000000000 ) ) ;
#12481 = EDGE_LOOP ( 'NONE', ( #9861, #19959, #15059, #19607 ) ) ;
#12482 = CIRCLE ( 'NONE', #6813, 0.05000000000000143219 ) ;
#12483 = VECTOR ( 'NONE', #6089, 1000.000000000000000 ) ;
#12484 = FACE_OUTER_BOUND ( 'NONE', #12519, .T. ) ;
#12485 = VECTOR ( 'NONE', #16144, 1000.000000000000000 ) ;
#12486 = CARTESIAN_POINT ( 'NONE',  ( 1.724728116533979616, 42.36054587065083155, 43.80876104995653719 ) ) ;
#12487 = ORIENTED_EDGE ( 'NONE', *, *, #9557, .F. ) ;
#12488 = VERTEX_POINT ( 'NONE', #9995 ) ;
#12489 = CARTESIAN_POINT ( 'NONE',  ( -21.92816239687475743, 42.46645089659918426, 13.74999999999999822 ) ) ;
#12490 = ADVANCED_FACE ( 'NONE', ( #6876 ), #20284, .F. ) ;
#12491 = LINE ( 'NONE', #21140, #5315 ) ;
#12492 = ORIENTED_EDGE ( 'NONE', *, *, #15931, .F. ) ;
#12493 = ORIENTED_EDGE ( 'NONE', *, *, #8146, .T. ) ;
#12494 = ADVANCED_FACE ( 'NONE', ( #13563 ), #8655, .F. ) ;
#12495 = AXIS2_PLACEMENT_3D ( 'NONE', #721, #2075, #17400 ) ;
#12496 = ADVANCED_FACE ( 'NONE', ( #4960 ), #8416, .F. ) ;
#12497 = AXIS2_PLACEMENT_3D ( 'NONE', #13619, #1421, #1637 ) ;
#12498 = ORIENTED_EDGE ( 'NONE', *, *, #202, .F. ) ;
#12499 = DIRECTION ( 'NONE',  ( -0.9729678061520319332, -0.2309407893632090258, 0.000000000000000000 ) ) ;
#12500 = AXIS2_PLACEMENT_3D ( 'NONE', #14446, #3615, #18711 ) ;
#12501 = EDGE_CURVE ( 'NONE', #17830, #7599, #19683, .T. ) ;
#12502 = CARTESIAN_POINT ( 'NONE',  ( -3.627054932750481964, -32.93424481021354921, 68.00000000000000000 ) ) ;
#12503 = EDGE_CURVE ( 'NONE', #21390, #1195, #2662, .T. ) ;
#12504 = CARTESIAN_POINT ( 'NONE',  ( -31.50000000000002132, -72.00000000000001421, 3.200000000000000178 ) ) ;
#12505 = DIRECTION ( 'NONE',  ( 1.000000000000000000, 0.000000000000000000, 0.000000000000000000 ) ) ;
#12506 = EDGE_LOOP ( 'NONE', ( #22101, #7048, #13753, #21676 ) ) ;
#12507 = DIRECTION ( 'NONE',  ( -1.224646799147353207E-16, -0.000000000000000000, -1.000000000000000000 ) ) ;
#12508 = DIRECTION ( 'NONE',  ( 0.000000000000000000, 0.000000000000000000, 1.000000000000000000 ) ) ;
#12509 = DIRECTION ( 'NONE',  ( 1.000000000000000000, 0.000000000000000000, -2.891205793294662451E-15 ) ) ;
#12510 = CIRCLE ( 'NONE', #4665, 0.2500000000000002220 ) ;
#12511 = EDGE_LOOP ( 'NONE', ( #5489, #2824, #10933, #17711 ) ) ;
#12512 = EDGE_CURVE ( 'NONE', #18203, #1535, #3526, .T. ) ;
#12513 = AXIS2_PLACEMENT_3D ( 'NONE', #5306, #3384, #29 ) ;
#12514 = EDGE_LOOP ( 'NONE', ( #14204, #11948, #7872, #3685 ) ) ;
#12515 = VERTEX_POINT ( 'NONE', #17247 ) ;
#12516 = ORIENTED_EDGE ( 'NONE', *, *, #4892, .F. ) ;
#12517 = CARTESIAN_POINT ( 'NONE',  ( -27.37540678000426908, 36.74634676501047181, 42.50000000000000000 ) ) ;
#12518 = ITEM_DEFINED_TRANSFORMATION ( 'NONE', 'NONE', #18343,  #17493 ) ;
#12519 = EDGE_LOOP ( 'NONE', ( #6214, #711, #21572, #8051 ) ) ;
#12520 = EDGE_LOOP ( 'NONE', ( #18050, #5620, #10099, #14894 ) ) ;
#12521 = CARTESIAN_POINT ( 'NONE',  ( 23.04897344237150492, -2.295898177910679738, 13.26544997878583487 ) ) ;
#12522 = ORIENTED_EDGE ( 'NONE', *, *, #16770, .F. ) ;
#12523 = CARTESIAN_POINT ( 'NONE',  ( -27.37540678000426908, 36.74634676501047181, 13.79999999999999893 ) ) ;
#12524 = ADVANCED_FACE ( 'NONE', ( #7611 ), #6756, .F. ) ;
#12525 = ADVANCED_FACE ( 'NONE', ( #13764 ), #18900, .F. ) ;
#12526 = LINE ( 'NONE', #14090, #13773 ) ;
#12527 = DIRECTION ( 'NONE',  ( 0.000000000000000000, 1.000000000000000000, -0.000000000000000000 ) ) ;
#12528 = CYLINDRICAL_SURFACE ( 'NONE', #13070, 3.017785046117004377 ) ;
#12529 = CIRCLE ( 'NONE', #11815, 0.2500000000000002220 ) ;
#12530 = DIRECTION ( 'NONE',  ( 0.000000000000000000, 0.000000000000000000, 1.000000000000000000 ) ) ;
#12531 = CARTESIAN_POINT ( 'NONE',  ( -3.627054932750481964, -33.43424481021354921, 42.50000000000000000 ) ) ;
#12532 = CARTESIAN_POINT ( 'NONE',  ( 30.49999999999999645, 70.29999999999999716, 0.3000000000000033751 ) ) ;
#12533 = FACE_OUTER_BOUND ( 'NONE', #10848, .T. ) ;
#12534 = CARTESIAN_POINT ( 'NONE',  ( -15.21174975910705207, -51.61873716947361856, 68.50000000000000000 ) ) ;
#12535 = CIRCLE ( 'NONE', #746, 0.2500000000000002220 ) ;
#12536 = ORIENTED_EDGE ( 'NONE', *, *, #6878, .T. ) ;
#12537 = EDGE_LOOP ( 'NONE', ( #8527, #3901, #17858, #9787 ) ) ;
#12538 = CARTESIAN_POINT ( 'NONE',  ( -14.96174975910705207, 41.81054587065082728, 13.75000000000000000 ) ) ;
#12539 = SHAPE_REPRESENTATION_RELATIONSHIP ( 'NONE' , 'NONE' ,  #10840, #7272 ) ;
#12540 = EDGE_CURVE ( 'NONE', #5820, #12166, #9241, .T. ) ;
#12541 = EDGE_LOOP ( 'NONE', ( #8581, #15155, #8328, #5007, #13951, #10204, #2597, #8863, #3576, #11061, #10648, #17727, #5031, #1888, #11080, #8578, #5938, #14417, #11971, #6005 ) ) ;
#12542 = EDGE_CURVE ( 'NONE', #6971, #9271, #17350, .T. ) ;
#12543 = VERTEX_POINT ( 'NONE', #4125 ) ;
#12544 = ORIENTED_EDGE ( 'NONE', *, *, #10731, .F. ) ;
#12545 = AXIS2_PLACEMENT_3D ( 'NONE', #17655, #12608, #19450 ) ;
#12546 = EDGE_CURVE ( 'NONE', #16141, #17257, #12835, .T. ) ;
#12547 = AXIS2_PLACEMENT_3D ( 'NONE', #3386, #15240, #20410 ) ;
#12548 = DIRECTION ( 'NONE',  ( 0.000000000000000000, 0.000000000000000000, 1.000000000000000000 ) ) ;
#12549 = CIRCLE ( 'NONE', #16114, 0.5000000000000000000 ) ;
#12550 = CARTESIAN_POINT ( 'NONE',  ( 26.63662752439704917, 3.061616997868386099E-16, 3.500000000000000000 ) ) ;
#12551 = ORIENTED_EDGE ( 'NONE', *, *, #7903, .T. ) ;
#12552 = LINE ( 'NONE', #14351, #21815 ) ;
#12553 = FACE_OUTER_BOUND ( 'NONE', #4925, .T. ) ;
#12554 = CARTESIAN_POINT ( 'NONE',  ( -14.96174975910705207, 42.31054587065082728, 13.75000000000000000 ) ) ;
#12555 = CARTESIAN_POINT ( 'NONE',  ( 15.21174975910706095, 52.00603550409435627, 13.50000000000000000 ) ) ;
#12556 = CARTESIAN_POINT ( 'NONE',  ( -15.21174975910705207, 52.39333383871510108, 13.50000000000000000 ) ) ;
#12557 = CARTESIAN_POINT ( 'NONE',  ( -25.37540678000427263, 67.24634676501045760, 13.50000000000000000 ) ) ;
#12558 = ORIENTED_EDGE ( 'NONE', *, *, #10481, .F. ) ;
#12559 = LINE ( 'NONE', #21315, #10414 ) ;
#12560 = DIRECTION ( 'NONE',  ( -1.000000000000000000, 0.000000000000000000, 0.000000000000000000 ) ) ;
#12561 = DIRECTION ( 'NONE',  ( 0.000000000000000000, 0.000000000000000000, -1.000000000000000000 ) ) ;
#12562 = ORIENTED_EDGE ( 'NONE', *, *, #18857, .T. ) ;
#12563 = EDGE_LOOP ( 'NONE', ( #20321, #6539, #6107, #14722 ) ) ;
#12564 = ORIENTED_EDGE ( 'NONE', *, *, #16978, .T. ) ;
#12565 = CARTESIAN_POINT ( 'NONE',  ( -30.79999999999999005, 70.00000000000001421, 1.500000000000000222 ) ) ;
#12566 = APPLICATION_CONTEXT ( 'automotive_design' ) ;
#12567 = TOROIDAL_SURFACE ( 'NONE', #13287, 2.299999999999993161, 0.2999999999999999889 ) ;
#12569 = ADVANCED_FACE ( 'NONE', ( #19565 ), #2560, .F. ) ;
#12568 = CARTESIAN_POINT ( 'NONE',  ( -1.724728116533986721, 43.26054587065083012, 31.75876104995653648 ) ) ;
#12570 = VERTEX_POINT ( 'NONE', #18944 ) ;
#12571 = CIRCLE ( 'NONE', #5457, 0.05000000000000143219 ) ;
#12572 = EDGE_CURVE ( 'NONE', #6219, #22005, #19246, .T. ) ;
#12573 = DIRECTION ( 'NONE',  ( 0.000000000000000000, -0.000000000000000000, 1.000000000000000000 ) ) ;
#12574 = ORIENTED_EDGE ( 'NONE', *, *, #21659, .T. ) ;
#12575 = CARTESIAN_POINT ( 'NONE',  ( 29.13662752439705272, 0.000000000000000000, 13.19999999999999929 ) ) ;
#12576 = DIRECTION ( 'NONE',  ( 0.000000000000000000, -0.000000000000000000, -1.000000000000000000 ) ) ;
#12577 = VECTOR ( 'NONE', #17801, 1000.000000000000000 ) ;
#12578 = VERTEX_POINT ( 'NONE', #6160 ) ;
#12579 = CARTESIAN_POINT ( 'NONE',  ( 3.127054932750481964, -33.43424481021354921, 68.00000000000000000 ) ) ;
#12580 = LINE ( 'NONE', #5691, #1722 ) ;
#12581 = DIRECTION ( 'NONE',  ( 0.000000000000000000, 1.000000000000000000, 0.000000000000000000 ) ) ;
#12582 = DIRECTION ( 'NONE',  ( -0.000000000000000000, -0.000000000000000000, 1.000000000000000000 ) ) ;
#12583 = ORIENTED_EDGE ( 'NONE', *, *, #19638, .F. ) ;
#12584 = CARTESIAN_POINT ( 'NONE',  ( 30.37540678000427619, 63.74634676501045050, 7.500000000000000000 ) ) ;
#12585 = CARTESIAN_POINT ( 'NONE',  ( -27.37540678000427619, 5.683640910026986681, 13.79999999999999893 ) ) ;
#12586 = DIRECTION ( 'NONE',  ( 1.000000000000000000, 0.000000000000000000, 0.000000000000000000 ) ) ;
#12587 = DIRECTION ( 'NONE',  ( -2.388292521039847891E-16, 0.000000000000000000, -1.000000000000000000 ) ) ;
#12588 = ORIENTED_EDGE ( 'NONE', *, *, #4233, .T. ) ;
#12589 = EDGE_CURVE ( 'NONE', #10528, #1711, #18222, .T. ) ;
#12590 = CARTESIAN_POINT ( 'NONE',  ( -35.00000000000000000, 85.00000000000000000, 0.000000000000000000 ) ) ;
#12591 = EDGE_LOOP ( 'NONE', ( #7752, #12064, #9111, #4720 ) ) ;
#12592 = CARTESIAN_POINT ( 'NONE',  ( 25.37540678000426908, 39.04634676501046187, 13.79999999999999893 ) ) ;
#12593 = CARTESIAN_POINT ( 'NONE',  ( -23.02398829872513986, -3.528912754968629439, 13.79999999999999893 ) ) ;
#12594 = ORIENTED_EDGE ( 'NONE', *, *, #21414, .F. ) ;
#12595 = ORIENTED_EDGE ( 'NONE', *, *, #11006, .T. ) ;
#12596 = FACE_OUTER_BOUND ( 'NONE', #20987, .T. ) ;
#12597 = ADVANCED_FACE ( 'NONE', ( #8268 ), #18550, .T. ) ;
#12598 = EDGE_CURVE ( 'NONE', #19220, #17187, #16631, .T. ) ;
#12599 = DIRECTION ( 'NONE',  ( -0.000000000000000000, 0.000000000000000000, 1.000000000000000000 ) ) ;
#12600 = VERTEX_POINT ( 'NONE', #1310 ) ;
#12601 = ORIENTED_EDGE ( 'NONE', *, *, #7856, .T. ) ;
#12602 = DIRECTION ( 'NONE',  ( 0.000000000000000000, 0.000000000000000000, 1.000000000000000000 ) ) ;
#12603 = CARTESIAN_POINT ( 'NONE',  ( -15.21174975910705207, 41.81054587065082728, 68.50000000000000000 ) ) ;
#12604 = DIRECTION ( 'NONE',  ( 0.000000000000000000, 0.000000000000000000, -1.000000000000000000 ) ) ;
#12605 = LINE ( 'NONE', #21251, #20111 ) ;
#12606 = DIRECTION ( 'NONE',  ( 0.000000000000000000, 0.000000000000000000, -1.000000000000000000 ) ) ;
#12607 = EDGE_CURVE ( 'NONE', #5056, #22136, #12946, .T. ) ;
#12608 = DIRECTION ( 'NONE',  ( -0.000000000000000000, 1.000000000000000000, 0.000000000000000000 ) ) ;
#12609 = DIRECTION ( 'NONE',  ( -1.000000000000000000, 0.000000000000000000, 0.000000000000000000 ) ) ;
#12610 = COLOUR_RGB ( '', 0.72549020, 0.75294118, 0.79215686) ;
#12611 = ORIENTED_EDGE ( 'NONE', *, *, #247, .T. ) ;
#12612 = DIRECTION ( 'NONE',  ( 0.000000000000000000, -1.000000000000000000, 0.000000000000000000 ) ) ;
#12613 = CARTESIAN_POINT ( 'NONE',  ( -14.96174975910705207, 51.61873716947361856, 68.00000000000000000 ) ) ;
#12614 = CARTESIAN_POINT ( 'NONE',  ( -23.49018890325625364, 45.04852366434393218, 13.74999999999999822 ) ) ;
#12615 = ORIENTED_EDGE ( 'NONE', *, *, #7693, .F. ) ;
#12616 = EDGE_CURVE ( 'NONE', #21319, #15844, #3160, .T. ) ;
#12617 = DIRECTION ( 'NONE',  ( -1.000000000000000000, 3.009265538104883829E-28, -4.336808689941893885E-15 ) ) ;
#12618 = EDGE_LOOP ( 'NONE', ( #10093, #1749, #18283, #16482 ) ) ;
#12619 = EDGE_CURVE ( 'NONE', #20520, #12192, #4246, .T. ) ;
#12620 = ORIENTED_EDGE ( 'NONE', *, *, #12297, .T. ) ;
#12621 = DIRECTION ( 'NONE',  ( 1.000000000000000000, 0.000000000000000000, 0.000000000000000000 ) ) ;
#12622 = ITEM_DEFINED_TRANSFORMATION ( 'NONE', 'NONE', #5150,  #17493 ) ;
#12623 = VERTEX_POINT ( 'NONE', #19793 ) ;
#12624 = ORIENTED_EDGE ( 'NONE', *, *, #1442, .T. ) ;
#12625 = PRODUCT_DEFINITION_FORMATION_WITH_SPECIFIED_SOURCE ( 'ANY', '', #13, .NOT_KNOWN. ) ;
#12626 = DIRECTION ( 'NONE',  ( 0.000000000000000000, -1.000000000000000000, 0.000000000000000000 ) ) ;
#12627 = ORIENTED_EDGE ( 'NONE', *, *, #12469, .F. ) ;
#12628 = LINE ( 'NONE', #14208, #1440 ) ;
#12629 = DIRECTION ( 'NONE',  ( 0.000000000000000000, 0.000000000000000000, -1.000000000000000000 ) ) ;
#12630 = ADVANCED_FACE ( 'NONE', ( #16531 ), #7837, .T. ) ;
#12631 = AXIS2_PLACEMENT_3D ( 'NONE', #7479, #14277, #21011 ) ;
#12632 = CARTESIAN_POINT ( 'NONE',  ( 1.724728116533979838, 42.36054587065083155, 33.66679706732590915 ) ) ;
#12633 = CARTESIAN_POINT ( 'NONE',  ( -9.141460742840918030, 33.43424481021354921, 7.321391277662001151 ) ) ;
#12634 = DIRECTION ( 'NONE',  ( 1.000000000000000000, 0.000000000000000000, 0.000000000000000000 ) ) ;
#12635 = CARTESIAN_POINT ( 'NONE',  ( 0.000000000000000000, 43.26054587065083012, 35.75876104995654003 ) ) ;
#12636 = LINE ( 'NONE', #9464, #14308 ) ;
#12637 = VECTOR ( 'NONE', #21895, 1000.000000000000000 ) ;
#12638 = ADVANCED_FACE ( 'NONE', ( #3002 ), #20231, .F. ) ;
#12639 = CARTESIAN_POINT ( 'NONE',  ( 23.02398829872513986, 7.027230193580998154E-15, 7.500000000000000000 ) ) ;
#12640 = ADVANCED_FACE ( 'NONE', ( #4456 ), #18327, .F. ) ;
#12641 = VERTEX_POINT ( 'NONE', #4907 ) ;
#12642 = EDGE_LOOP ( 'NONE', ( #19257, #2674, #3363, #9444 ) ) ;
#12643 = DIRECTION ( 'NONE',  ( 1.000000000000000000, 0.000000000000000000, 0.000000000000000000 ) ) ;
#12644 = EDGE_CURVE ( 'NONE', #1806, #3604, #12429, .T. ) ;
#12645 = ORIENTED_EDGE ( 'NONE', *, *, #12758, .F. ) ;
#12646 = ORIENTED_EDGE ( 'NONE', *, *, #20339, .T. ) ;
#12647 = AXIS2_PLACEMENT_3D ( 'NONE', #7865, #684, #14661 ) ;
#12648 = CARTESIAN_POINT ( 'NONE',  ( -1.774728116533986766, 43.31054587065082728, 45.66679706732590205 ) ) ;
#12649 = DIRECTION ( 'NONE',  ( -0.000000000000000000, 1.000000000000000000, -0.000000000000000000 ) ) ;
#12650 = ORIENTED_EDGE ( 'NONE', *, *, #15662, .F. ) ;
#12651 = DIRECTION ( 'NONE',  ( -1.000000000000000000, -2.891205793294662451E-15, 0.000000000000000000 ) ) ;
#12652 = EDGE_CURVE ( 'NONE', #4334, #18447, #6419, .T. ) ;
#12653 = CARTESIAN_POINT ( 'NONE',  ( 17.95292532278785913, -50.11873716947361856, 68.00000000000000000 ) ) ;
#12654 = CARTESIAN_POINT ( 'NONE',  ( 14.96512931750545938, 51.87344388792876515, 13.83591901640606459 ) ) ;
#12655 = FACE_OUTER_BOUND ( 'NONE', #5299, .T. ) ;
#12656 = CARTESIAN_POINT ( 'NONE',  ( -17.93704824106378837, 50.11873716947361856, 13.87500000000000000 ) ) ;
#12657 = EDGE_LOOP ( 'NONE', ( #13530, #16277, #20373, #15981 ) ) ;
#12658 = DIRECTION ( 'NONE',  ( 0.000000000000000000, 0.000000000000000000, 1.000000000000000000 ) ) ;
#12659 = DIRECTION ( 'NONE',  ( -0.000000000000000000, 1.000000000000000000, -0.000000000000000000 ) ) ;
#12660 = DIRECTION ( 'NONE',  ( 0.000000000000000000, 1.000000000000000000, 0.000000000000000000 ) ) ;
#12661 = EDGE_LOOP ( 'NONE', ( #2188, #218, #3513, #3907 ) ) ;
#12662 = CIRCLE ( 'NONE', #16967, 0.2999999999999999334 ) ;
#12663 = ORIENTED_EDGE ( 'NONE', *, *, #19576, .F. ) ;
#12664 = AXIS2_PLACEMENT_3D ( 'NONE', #8271, #1648, #21926 ) ;
#12665 = ORIENTED_EDGE ( 'NONE', *, *, #9851, .F. ) ;
#12666 = DIRECTION ( 'NONE',  ( -3.052134192567367925E-16, 1.000000000000000000, 0.000000000000000000 ) ) ;
#12667 = EDGE_CURVE ( 'NONE', #2503, #18174, #11268, .T. ) ;
#12668 = LINE ( 'NONE', #21438, #14180 ) ;
#12669 = CARTESIAN_POINT ( 'NONE',  ( 29.37540678000427619, -5.299999999999999822, 7.500000000000000000 ) ) ;
#12670 = VERTEX_POINT ( 'NONE', #14747 ) ;
#12671 = CYLINDRICAL_SURFACE ( 'NONE', #20402, 0.5000000000000004441 ) ;
#12672 = AXIS2_PLACEMENT_3D ( 'NONE', #5105, #61, #6912 ) ;
#12673 = DIRECTION ( 'NONE',  ( 0.000000000000000000, 0.000000000000000000, 1.000000000000000000 ) ) ;
#12674 = DIRECTION ( 'NONE',  ( 0.000000000000000000, -1.000000000000000000, 0.000000000000000000 ) ) ;
#12675 = CARTESIAN_POINT ( 'NONE',  ( -27.37540678000427619, 10.94079601157914539, 13.79999999999999893 ) ) ;
#12676 = AXIS2_PLACEMENT_3D ( 'NONE', #11575, #22133, #13370 ) ;
#12677 = DIRECTION ( 'NONE',  ( 0.000000000000000000, -1.000000000000000000, 0.000000000000000000 ) ) ;
#12678 = DIRECTION ( 'NONE',  ( -1.000000000000000000, 0.000000000000000000, -0.000000000000000000 ) ) ;
#12679 = CIRCLE ( 'NONE', #6657, 0.5000000000000004441 ) ;
#12680 = ORIENTED_EDGE ( 'NONE', *, *, #10020, .T. ) ;
#12681 = DIRECTION ( 'NONE',  ( 1.000000000000000000, 0.000000000000000000, 0.000000000000000000 ) ) ;
#12682 = EDGE_CURVE ( 'NONE', #10568, #17690, #9619, .T. ) ;
#12683 = DIRECTION ( 'NONE',  ( -1.734723475976806848E-16, 0.000000000000000000, 1.000000000000000000 ) ) ;
#12684 = DIRECTION ( 'NONE',  ( 1.000000000000000000, 0.000000000000000000, 0.000000000000000000 ) ) ;
#12685 = ORIENTED_EDGE ( 'NONE', *, *, #12546, .F. ) ;
#12686 = EDGE_CURVE ( 'NONE', #497, #16854, #19911, .T. ) ;
#12687 = LINE ( 'NONE', #9703, #20205 ) ;
#12688 = ORIENTED_EDGE ( 'NONE', *, *, #543, .T. ) ;
#12689 = CARTESIAN_POINT ( 'NONE',  ( -1.824728116533986810, 42.36054587065083155, 45.76679706732590347 ) ) ;
#12690 = CARTESIAN_POINT ( 'NONE',  ( 34.39999999999998437, 84.70000000000001705, 0.6000000000000041966 ) ) ;
#12691 = ORIENTED_EDGE ( 'NONE', *, *, #15088, .T. ) ;
#12692 = CIRCLE ( 'NONE', #20234, 1.999999999999991340 ) ;
#12693 = VECTOR ( 'NONE', #3379, 1000.000000000000000 ) ;
#12694 = ORIENTED_EDGE ( 'NONE', *, *, #12540, .F. ) ;
#12695 = CARTESIAN_POINT ( 'NONE',  ( -14.98285978764165449, 51.83353206222920306, 13.49999999999971756 ) ) ;
#12696 = CARTESIAN_POINT ( 'NONE',  ( 1.724728116533979838, 43.31054587065082728, 41.66679706732590915 ) ) ;
#12697 = CARTESIAN_POINT ( 'NONE',  ( 14.96174975910705918, 32.10873716947361345, 13.79999999999999893 ) ) ;
#12698 = AXIS2_PLACEMENT_3D ( 'NONE', #708, #14580, #2391 ) ;
#12699 = ORIENTED_EDGE ( 'NONE', *, *, #14950, .F. ) ;
#12700 = CIRCLE ( 'NONE', #15565, 0.5999999999999998668 ) ;
#12701 = ORIENTED_EDGE ( 'NONE', *, *, #14050, .F. ) ;
#12702 = EDGE_CURVE ( 'NONE', #1070, #14169, #11394, .T. ) ;
#12703 = EDGE_CURVE ( 'NONE', #17559, #19232, #12443, .T. ) ;
#12704 = ORIENTED_EDGE ( 'NONE', *, *, #1073, .F. ) ;
#12705 = LINE ( 'NONE', #19558, #15629 ) ;
#12706 = CIRCLE ( 'NONE', #22034, 0.6999999999999992895 ) ;
#12707 = TOROIDAL_SURFACE ( 'NONE', #20622, 1.300000000000000044, 0.2999999999999999889 ) ;
#12708 = CARTESIAN_POINT ( 'NONE',  ( 15.95292532278785913, -51.61873716947361856, 68.00000000000000000 ) ) ;
#12709 = TOROIDAL_SURFACE ( 'NONE', #3089, 0.2500000000000000000, 0.2500000000000000000 ) ;
#12710 = CARTESIAN_POINT ( 'NONE',  ( -23.36959064016851073, 45.26242829375641463, 13.74999999999999822 ) ) ;
#12711 = DIRECTION ( 'NONE',  ( -0.9729678061520345977, -0.2309407893631976461, 0.000000000000000000 ) ) ;
#12712 = ADVANCED_FACE ( 'NONE', ( #10160 ), #12154, .F. ) ;
#12713 = LINE ( 'NONE', #11060, #5977 ) ;
#12714 = VERTEX_POINT ( 'NONE', #3568 ) ;
#12715 = DIRECTION ( 'NONE',  ( 1.000000000000000000, 0.000000000000000000, 0.000000000000000000 ) ) ;
#12716 = AXIS2_PLACEMENT_3D ( 'NONE', #4275, #7537, #9311 ) ;
#12717 = CYLINDRICAL_SURFACE ( 'NONE', #13898, 0.1000000000000028644 ) ;
#12718 = CARTESIAN_POINT ( 'NONE',  ( 34.39999999999998437, 85.00000000000000000, 0.6000000000000041966 ) ) ;
#12719 = DIRECTION ( 'NONE',  ( 0.4461977533474359991, 1.557891129246304494E-15, -0.8949343913984425525 ) ) ;
#12720 = DIRECTION ( 'NONE',  ( -6.751320378806396803E-15, -1.602473635475851075E-15, 1.000000000000000000 ) ) ;
#12721 = ORIENTED_EDGE ( 'NONE', *, *, #3746, .F. ) ;
#12722 = AXIS2_PLACEMENT_3D ( 'NONE', #7466, #5891, #4091 ) ;
#12723 = AXIS2_PLACEMENT_3D ( 'NONE', #16939, #3305, #1504 ) ;
#12724 = AXIS2_PLACEMENT_3D ( 'NONE', #10895, #9110, #21740 ) ;
#12725 = ORIENTED_EDGE ( 'NONE', *, *, #6209, .T. ) ;
#12726 = ORIENTED_EDGE ( 'NONE', *, *, #1669, .F. ) ;
#12727 = DIRECTION ( 'NONE',  ( 0.000000000000000000, 0.000000000000000000, 1.000000000000000000 ) ) ;
#12728 = ITEM_DEFINED_TRANSFORMATION ( 'NONE', 'NONE', #6602,  #17493 ) ;
#12729 = ADVANCED_FACE ( 'NONE', ( #5134 ), #8610, .T. ) ;
#12730 = EDGE_LOOP ( 'NONE', ( #19776, #963, #16538, #1524 ) ) ;
#12731 = ORIENTED_EDGE ( 'NONE', *, *, #8031, .T. ) ;
#12732 = VECTOR ( 'NONE', #821, 1000.000000000000000 ) ;
#12733 = DIRECTION ( 'NONE',  ( 2.832483164223434527E-16, -1.000000000000000000, -0.000000000000000000 ) ) ;
#12734 = VERTEX_POINT ( 'NONE', #3675 ) ;
#12735 = DIRECTION ( 'NONE',  ( 1.000000000000000000, -0.000000000000000000, 0.000000000000000000 ) ) ;
#12736 = B_SPLINE_CURVE_WITH_KNOTS ( 'NONE', 3,
 ( #21576, #16064, #9708, #2758, #21238, #11146, #16511, #2430, #9595, #12593 ),
 .UNSPECIFIED., .F., .F.,
 ( 4, 2, 2, 2, 4 ),
 ( 0.000000000000000000, 0.0001998921237118768868, 0.0003997842474237537735, 0.0007995684948475064628, 0.001599136989695014444 ),
 .UNSPECIFIED. ) ;
#12737 = EDGE_CURVE ( 'NONE', #630, #4678, #10494, .T. ) ;
#12738 = DIRECTION ( 'NONE',  ( 0.000000000000000000, 0.000000000000000000, 1.000000000000000000 ) ) ;
#12739 = DIRECTION ( 'NONE',  ( 0.000000000000000000, 1.000000000000000000, 0.000000000000000000 ) ) ;
#12740 = DIRECTION ( 'NONE',  ( 0.000000000000000000, 0.000000000000000000, 1.000000000000000000 ) ) ;
#12741 = AXIS2_PLACEMENT_3D ( 'NONE', #13330, #20168, #3169 ) ;
#12742 = ADVANCED_FACE ( 'NONE', ( #8490 ), #298, .F. ) ;
#12743 = CIRCLE ( 'NONE', #3125, 3.500000000000003109 ) ;
#12744 = AXIS2_PLACEMENT_3D ( 'NONE', #19358, #2232, #9062 ) ;
#12745 = DIRECTION ( 'NONE',  ( 0.000000000000000000, 0.000000000000000000, 1.000000000000000000 ) ) ;
#12746 = VECTOR ( 'NONE', #18413, 1000.000000000000000 ) ;
#12747 = CARTESIAN_POINT ( 'NONE',  ( 29.20000000000002061, 50.00000000000000000, 0.000000000000000000 ) ) ;
#12748 = CARTESIAN_POINT ( 'NONE',  ( -33.80000000000001847, 85.00000000000000000, 78.20000000000000284 ) ) ;
#12749 = DIRECTION ( 'NONE',  ( 0.000000000000000000, 0.000000000000000000, 1.000000000000000000 ) ) ;
#12750 = AXIS2_PLACEMENT_3D ( 'NONE', #18254, #9656, #2823 ) ;
#12751 = B_SPLINE_CURVE_WITH_KNOTS ( 'NONE', 3,
 ( #3293, #8558, #20419, #15367, #19982, #16584, #8331, #6446 ),
 .UNSPECIFIED., .F., .F.,
 ( 4, 2, 2, 4 ),
 ( -3.464559252384133923E-06, 0.0002895415592466213275, 0.0004360446184961240686, 0.0005825476777456268639 ),
 .UNSPECIFIED. ) ;
#12752 = CARTESIAN_POINT ( 'NONE',  ( -1.724728116533986721, 42.36054587065083155, 39.80876104995653719 ) ) ;
#12753 = LINE ( 'NONE', #3756, #278 ) ;
#12754 = ORIENTED_EDGE ( 'NONE', *, *, #18214, .F. ) ;
#12755 = VERTEX_POINT ( 'NONE', #18895 ) ;
#12756 = CYLINDRICAL_SURFACE ( 'NONE', #15299, 0.2999999999999999334 ) ;
#12757 =( NAMED_UNIT ( * ) PLANE_ANGLE_UNIT ( ) SI_UNIT ( $, .RADIAN. ) );
#12758 = EDGE_CURVE ( 'NONE', #1150, #5485, #4615, .T. ) ;
#12759 = ORIENTED_EDGE ( 'NONE', *, *, #3524, .T. ) ;
#12760 = EDGE_LOOP ( 'NONE', ( #7982, #6569, #5010, #13435 ) ) ;
#12761 = CIRCLE ( 'NONE', #17427, 2.800000000000003819 ) ;
#12762 = CIRCLE ( 'NONE', #18495, 0.05000000000000143219 ) ;
#12763 = VECTOR ( 'NONE', #19670, 1000.000000000000000 ) ;
#12764 = ORIENTED_EDGE ( 'NONE', *, *, #6167, .F. ) ;
#12765 = AXIS2_PLACEMENT_3D ( 'NONE', #6515, #16993, #20593 ) ;
#12766 = VECTOR ( 'NONE', #7978, 1000.000000000000000 ) ;
#12767 = AXIS2_PLACEMENT_3D ( 'NONE', #16116, #10576, #10375 ) ;
#12768 = EDGE_CURVE ( 'NONE', #5602, #12260, #13183, .T. ) ;
#12769 = CARTESIAN_POINT ( 'NONE',  ( -15.21174975910705207, -52.39333383871510108, 13.50000000000000000 ) ) ;
#12770 = EDGE_CURVE ( 'NONE', #5113, #18383, #13535, .T. ) ;
#12771 = CARTESIAN_POINT ( 'NONE',  ( 23.02398829872513986, 5.683640910026983128, 13.79999999999999893 ) ) ;
#12772 = ORIENTED_EDGE ( 'NONE', *, *, #13410, .F. ) ;
#12773 = CARTESIAN_POINT ( 'NONE',  ( 17.92752199202933738, -38.74634676501045760, 13.62426406871192874 ) ) ;
#12774 = ADVANCED_FACE ( 'NONE', ( #6832 ), #14971, .T. ) ;
#12775 = DIRECTION ( 'NONE',  ( -1.000000000000000000, 0.000000000000000000, 0.000000000000000000 ) ) ;
#12776 = CARTESIAN_POINT ( 'NONE',  ( 14.66918479711007706, 51.92478806352735887, 13.50000000000000000 ) ) ;
#12777 = CARTESIAN_POINT ( 'NONE',  ( -26.37540678000427619, -10.94079601157914716, 13.79999999999999893 ) ) ;
#12778 = AXIS2_PLACEMENT_3D ( 'NONE', #16154, #17844, #5464 ) ;
#12779 = AXIS2_PLACEMENT_3D ( 'NONE', #14402, #10945, #7505 ) ;
#12780 = FACE_OUTER_BOUND ( 'NONE', #9401, .T. ) ;
#12781 = ORIENTED_EDGE ( 'NONE', *, *, #9342, .T. ) ;
#12782 = DIRECTION ( 'NONE',  ( 1.000000000000000000, -0.000000000000000000, 0.000000000000000000 ) ) ;
#12783 = CYLINDRICAL_SURFACE ( 'NONE', #10221, 0.09999999999999939493 ) ;
#12784 = AXIS2_PLACEMENT_3D ( 'NONE', #12475, #12251, #6934 ) ;
#12785 = CYLINDRICAL_SURFACE ( 'NONE', #17761, 0.5000000000000000000 ) ;
#12786 = ORIENTED_EDGE ( 'NONE', *, *, #5145, .T. ) ;
#12787 = VERTEX_POINT ( 'NONE', #13624 ) ;
#12788 = AXIS2_PLACEMENT_3D ( 'NONE', #19363, #5396, #541 ) ;
#12789 = ORIENTED_EDGE ( 'NONE', *, *, #1999, .F. ) ;
#12790 = CIRCLE ( 'NONE', #6040, 0.05000000000000143219 ) ;
#12791 = DIRECTION ( 'NONE',  ( 0.000000000000000000, -0.000000000000000000, -1.000000000000000000 ) ) ;
#12792 = ADVANCED_FACE ( 'NONE', ( #182 ), #11825, .F. ) ;
#12793 = VERTEX_POINT ( 'NONE', #3338 ) ;
#12794 = LINE ( 'NONE', #19751, #17413 ) ;
#12795 = ORIENTED_EDGE ( 'NONE', *, *, #7736, .F. ) ;
#12796 = DIRECTION ( 'NONE',  ( 0.000000000000000000, 0.000000000000000000, -1.000000000000000000 ) ) ;
#12797 = AXIS2_PLACEMENT_3D ( 'NONE', #17100, #13513, #92 ) ;
#12798 = FACE_OUTER_BOUND ( 'NONE', #3706, .T. ) ;
#12799 = DIRECTION ( 'NONE',  ( 0.000000000000000000, 0.000000000000000000, -1.000000000000000000 ) ) ;
#12800 = EDGE_CURVE ( 'NONE', #14491, #10431, #6771, .T. ) ;
#12801 = CARTESIAN_POINT ( 'NONE',  ( 1.724728116533979616, 43.26054587065083012, 51.75876104995654003 ) ) ;
#12802 = DIRECTION ( 'NONE',  ( 1.734723475976806848E-16, -0.000000000000000000, -1.000000000000000000 ) ) ;
#12803 = ORIENTED_EDGE ( 'NONE', *, *, #5455, .T. ) ;
#12804 = DIRECTION ( 'NONE',  ( 1.000000000000000000, 0.000000000000000000, 0.000000000000000000 ) ) ;
#12805 = AXIS2_PLACEMENT_3D ( 'NONE', #22162, #6838, #13953 ) ;
#12806 = EDGE_CURVE ( 'NONE', #16971, #17841, #18915, .T. ) ;
#12807 = CARTESIAN_POINT ( 'NONE',  ( 14.96174975910707161, 51.61873716947361856, 68.00000000000000000 ) ) ;
#12808 = CARTESIAN_POINT ( 'NONE',  ( 17.92752199202934094, -38.74634676501045760, 13.79999999999999893 ) ) ;
#12809 = CARTESIAN_POINT ( 'NONE',  ( -23.07454441928563682, -2.431172533959871096, 13.33570496075367728 ) ) ;
#12810 = ORIENTED_EDGE ( 'NONE', *, *, #21406, .T. ) ;
#12811 = LINE ( 'NONE', #4330, #7519 ) ;
#12812 = EDGE_LOOP ( 'NONE', ( #17592, #11941, #16555, #4626 ) ) ;
#12813 = DIRECTION ( 'NONE',  ( 1.000000000000000000, -0.000000000000000000, 0.000000000000000000 ) ) ;
#12814 = DIRECTION ( 'NONE',  ( 0.000000000000000000, 0.000000000000000000, -1.000000000000000000 ) ) ;
#12815 = ORIENTED_EDGE ( 'NONE', *, *, #8795, .T. ) ;
#12816 = ORIENTED_EDGE ( 'NONE', *, *, #4061, .F. ) ;
#12817 = CARTESIAN_POINT ( 'NONE',  ( -9.141460742840918030, 32.11873716947361856, 68.00000000000000000 ) ) ;
#12818 = DIRECTION ( 'NONE',  ( 0.000000000000000000, -1.000000000000000000, 0.000000000000000000 ) ) ;
#12819 = AXIS2_PLACEMENT_3D ( 'NONE', #6284, #2922, #8190 ) ;
#12820 = ORIENTED_EDGE ( 'NONE', *, *, #1016, .T. ) ;
#12821 = AXIS2_PLACEMENT_3D ( 'NONE', #17658, #15651, #2333 ) ;
#12822 = ADVANCED_FACE ( 'NONE', ( #10281 ), #5474, .T. ) ;
#12823 = EDGE_CURVE ( 'NONE', #1195, #20955, #15417, .T. ) ;
#12824 = EDGE_LOOP ( 'NONE', ( #10779, #18969, #17972, #3903 ) ) ;
#12825 = CARTESIAN_POINT ( 'NONE',  ( 34.39999999999998437, -85.00000000000000000, 79.69999999999998863 ) ) ;
#12826 = ORIENTED_EDGE ( 'NONE', *, *, #10966, .F. ) ;
#12827 = CARTESIAN_POINT ( 'NONE',  ( 1.724728116533979838, 43.31054587065082728, 37.71679706732590631 ) ) ;
#12828 = CARTESIAN_POINT ( 'NONE',  ( -25.37540678000427263, 63.74634676501045050, 13.50000000000000000 ) ) ;
#12829 = CARTESIAN_POINT ( 'NONE',  ( 1.724728116533979838, 42.31054587065082728, 41.66679706732590915 ) ) ;
#12830 = DIRECTION ( 'NONE',  ( 0.000000000000000000, -1.000000000000000000, 0.000000000000000000 ) ) ;
#12831 = CIRCLE ( 'NONE', #5005, 0.2500000000000002220 ) ;
#12832 =( GEOMETRIC_REPRESENTATION_CONTEXT ( 3 ) GLOBAL_UNCERTAINTY_ASSIGNED_CONTEXT ( ( #9765 ) ) GLOBAL_UNIT_ASSIGNED_CONTEXT ( ( #9986, #18591, #13661 ) ) REPRESENTATION_CONTEXT ( 'NONE', 'WORKASPACE' ) );
#12833 = VECTOR ( 'NONE', #12174, 1000.000000000000000 ) ;
#12834 = DIRECTION ( 'NONE',  ( -0.000000000000000000, -1.000000000000000000, -0.000000000000000000 ) ) ;
#12835 = LINE ( 'NONE', #9488, #2077 ) ;
#12836 = ORIENTED_EDGE ( 'NONE', *, *, #1768, .F. ) ;
#12837 = DIRECTION ( 'NONE',  ( 0.000000000000000000, 0.000000000000000000, 1.000000000000000000 ) ) ;
#12838 = DIRECTION ( 'NONE',  ( -1.000000000000000000, 0.000000000000000000, -0.000000000000000000 ) ) ;
#12839 = DIRECTION ( 'NONE',  ( 0.000000000000000000, 0.000000000000000000, 1.000000000000000000 ) ) ;
#12840 = FACE_OUTER_BOUND ( 'NONE', #12882, .T. ) ;
#12841 = LINE ( 'NONE', #6273, #21730 ) ;
#12842 = VERTEX_POINT ( 'NONE', #6939 ) ;
#12843 = ORIENTED_EDGE ( 'NONE', *, *, #14455, .T. ) ;
#12844 = DIRECTION ( 'NONE',  ( -0.000000000000000000, -0.000000000000000000, 1.000000000000000000 ) ) ;
#12845 = SHAPE_DEFINITION_REPRESENTATION ( #8045, #9142 ) ;
#12846 = CIRCLE ( 'NONE', #5376, 0.2999999999999999334 ) ;
#12847 = CIRCLE ( 'NONE', #8944, 0.1000000000000028644 ) ;
#12848 = ORIENTED_EDGE ( 'NONE', *, *, #6935, .F. ) ;
#12849 = VERTEX_POINT ( 'NONE', #22032 ) ;
#12851 = ADVANCED_FACE ( 'NONE', ( #7584 ), #15734, .F. ) ;
#12850 = SHAPE_REPRESENTATION ( 'Lampshade', ( #17493 ), #5511 ) ;
#12852 = FACE_OUTER_BOUND ( 'NONE', #15542, .T. ) ;
#12853 = VERTEX_POINT ( 'NONE', #7480 ) ;
#12854 = DIRECTION ( 'NONE',  ( -1.000000000000000000, -0.000000000000000000, -0.000000000000000000 ) ) ;
#12855 = ORIENTED_EDGE ( 'NONE', *, *, #5375, .F. ) ;
#12856 = LINE ( 'NONE', #19703, #9872 ) ;
#12857 = CARTESIAN_POINT ( 'NONE',  ( 4.985331397971318523, 42.46645089659917716, 69.50000000000000000 ) ) ;
#12858 = FACE_OUTER_BOUND ( 'NONE', #19695, .T. ) ;
#12859 = LINE ( 'NONE', #17903, #4683 ) ;
#12860 = CIRCLE ( 'NONE', #7531, 2.500000000000002220 ) ;
#12861 = CIRCLE ( 'NONE', #6472, 0.2499999999999977796 ) ;
#12862 = DIRECTION ( 'NONE',  ( 1.000000000000000000, 0.000000000000000000, 0.000000000000000000 ) ) ;
#12863 = CARTESIAN_POINT ( 'NONE',  ( 3.127054932750481964, -32.11873716947361856, 109.6002446535588319 ) ) ;
#12865 = ADVANCED_FACE ( 'NONE', ( #735 ), #5900, .T. ) ;
#12864 = DIRECTION ( 'NONE',  ( 1.000000000000000000, -1.038507728162729222E-16, -1.357958710150075923E-16 ) ) ;
#12866 = DIRECTION ( 'NONE',  ( 1.000000000000000000, 0.000000000000000000, 0.000000000000000000 ) ) ;
#12867 = VERTEX_POINT ( 'NONE', #17740 ) ;
#12868 = LINE ( 'NONE', #12639, #221 ) ;
#12869 = LINE ( 'NONE', #6194, #16711 ) ;
#12870 = EDGE_LOOP ( 'NONE', ( #13838, #13392, #21240, #7905 ) ) ;
#12871 = ORIENTED_EDGE ( 'NONE', *, *, #14245, .F. ) ;
#12872 = CARTESIAN_POINT ( 'NONE',  ( -8.638906393579159015, 43.51045099701597962, 68.06527860057354928 ) ) ;
#12873 = EDGE_CURVE ( 'NONE', #12977, #15569, #7488, .T. ) ;
#12874 =( LENGTH_UNIT ( ) NAMED_UNIT ( * ) SI_UNIT ( .MILLI., .METRE. ) );
#12875 = EDGE_CURVE ( 'NONE', #18789, #10528, #21409, .T. ) ;
#12876 = ORIENTED_EDGE ( 'NONE', *, *, #1332, .F. ) ;
#12877 = VERTEX_POINT ( 'NONE', #21341 ) ;
#12878 = ORIENTED_EDGE ( 'NONE', *, *, #9991, .T. ) ;
#12879 = VECTOR ( 'NONE', #11256, 1000.000000000000000 ) ;
#12880 = DIRECTION ( 'NONE',  ( -1.000000000000000000, 0.000000000000000000, 0.000000000000000000 ) ) ;
#12881 = CARTESIAN_POINT ( 'NONE',  ( -27.37540678000427974, -5.683640910026986681, 42.50000000000000000 ) ) ;
#12882 = EDGE_LOOP ( 'NONE', ( #9953, #17509, #8716, #2825 ) ) ;
#12883 = DIRECTION ( 'NONE',  ( 0.000000000000000000, 1.000000000000000000, -0.000000000000000000 ) ) ;
#12884 = EDGE_CURVE ( 'NONE', #17036, #1458, #16054, .T. ) ;
#12885 =( GEOMETRIC_REPRESENTATION_CONTEXT ( 3 ) GLOBAL_UNCERTAINTY_ASSIGNED_CONTEXT ( ( #6425 ) ) GLOBAL_UNIT_ASSIGNED_CONTEXT ( ( #8577, #13479, #13915 ) ) REPRESENTATION_CONTEXT ( 'NONE', 'WORKASPACE' ) );
#12886 = CARTESIAN_POINT ( 'NONE',  ( 23.32398829872514057, 7.118794219358020148E-15, 13.79999999999999893 ) ) ;
#12887 = CIRCLE ( 'NONE', #1839, 0.2999999999999999334 ) ;
#12888 = CARTESIAN_POINT ( 'NONE',  ( 1.724728116533979838, 43.26054587065083012, 45.66679706732590205 ) ) ;
#12889 = DIRECTION ( 'NONE',  ( -0.000000000000000000, -0.000000000000000000, -1.000000000000000000 ) ) ;
#12890 = CARTESIAN_POINT ( 'NONE',  ( -17.95292532278785913, 0.000000000000000000, 109.6002446535588319 ) ) ;
#12891 = ORIENTED_EDGE ( 'NONE', *, *, #10323, .T. ) ;
#12892 = DIRECTION ( 'NONE',  ( 1.000000000000000000, 0.000000000000000000, -2.388292521039847891E-16 ) ) ;
#12893 = CIRCLE ( 'NONE', #2141, 0.2500000000000002220 ) ;
#12894 = LINE ( 'NONE', #14357, #7026 ) ;
#12895 = EDGE_LOOP ( 'NONE', ( #19410, #15538, #1503, #16570, #12335, #18119 ) ) ;
#12896 = ORIENTED_EDGE ( 'NONE', *, *, #6065, .T. ) ;
#12897 = ORIENTED_EDGE ( 'NONE', *, *, #4048, .T. ) ;
#12898 = DIRECTION ( 'NONE',  ( 0.000000000000000000, -1.000000000000000000, 0.000000000000000000 ) ) ;
#12899 = DIRECTION ( 'NONE',  ( 1.000000000000000000, 0.000000000000000000, 0.000000000000000000 ) ) ;
#12900 = EDGE_CURVE ( 'NONE', #10497, #18203, #7256, .T. ) ;
#12901 = ORIENTED_EDGE ( 'NONE', *, *, #5963, .T. ) ;
#12902 = AXIS2_PLACEMENT_3D ( 'NONE', #17819, #5438, #12225 ) ;
#12903 = EDGE_CURVE ( 'NONE', #18309, #16692, #670, .T. ) ;
#12904 = DIRECTION ( 'NONE',  ( -1.000000000000000000, 0.000000000000000000, 2.107255972849994642E-16 ) ) ;
#12905 = EDGE_CURVE ( 'NONE', #5035, #2663, #3176, .T. ) ;
#12906 = AXIS2_PLACEMENT_3D ( 'NONE', #1483, #18489, #31 ) ;
#12907 = AXIS2_PLACEMENT_3D ( 'NONE', #1707, #1922, #11775 ) ;
#12908 = ORIENTED_EDGE ( 'NONE', *, *, #1173, .T. ) ;
#12909 = CARTESIAN_POINT ( 'NONE',  ( -1.724728116533986721, 42.36054587065083155, 33.66679706732590915 ) ) ;
#12910 = CARTESIAN_POINT ( 'NONE',  ( 1.824728116533979705, 43.31054587065082728, 41.66679706732590915 ) ) ;
#12911 = DIRECTION ( 'NONE',  ( -1.000000000000000000, 0.000000000000000000, 0.000000000000000000 ) ) ;
#12912 = FACE_OUTER_BOUND ( 'NONE', #13122, .T. ) ;
#12913 = CARTESIAN_POINT ( 'NONE',  ( -3.127054932750481964, -32.61873716947361856, 109.6002446535588319 ) ) ;
#12914 = DIRECTION ( 'NONE',  ( 0.000000000000000000, -1.000000000000000000, 0.000000000000000000 ) ) ;
#12915 = ORIENTED_EDGE ( 'NONE', *, *, #6092, .T. ) ;
#12916 = DIRECTION ( 'NONE',  ( 0.000000000000000000, 0.000000000000000000, 1.000000000000000000 ) ) ;
#12917 = CARTESIAN_POINT ( 'NONE',  ( 1.824728116533979261, 43.31054587065082728, 43.80876104995653719 ) ) ;
#12918 = EDGE_CURVE ( 'NONE', #11228, #19966, #14053, .T. ) ;
#12919 = CARTESIAN_POINT ( 'NONE',  ( 3.627054932750481964, -32.93424481021354921, 68.00000000000000000 ) ) ;
#12920 = CYLINDRICAL_SURFACE ( 'NONE', #6867, 0.2999999999999999334 ) ;
#12921 = ORIENTED_EDGE ( 'NONE', *, *, #17329, .T. ) ;
#12922 = DIRECTION ( 'NONE',  ( 1.000000000000000000, -3.052134192567374827E-16, 0.000000000000000000 ) ) ;
#12923 = DIRECTION ( 'NONE',  ( -1.000000000000000000, 0.000000000000000000, 0.000000000000000000 ) ) ;
#12924 = AXIS2_PLACEMENT_3D ( 'NONE', #5855, #12301, #19154 ) ;
#12925 = ORIENTED_EDGE ( 'NONE', *, *, #983, .T. ) ;
#12926 = CARTESIAN_POINT ( 'NONE',  ( -14.96174975910705207, 41.81054587065082728, 68.25000000000000000 ) ) ;
#12927 = VECTOR ( 'NONE', #16752, 1000.000000000000000 ) ;
#12928 = DIRECTION ( 'NONE',  ( 0.000000000000000000, 0.000000000000000000, 1.000000000000000000 ) ) ;
#12929 = EDGE_LOOP ( 'NONE', ( #15659, #15107, #12781, #1052, #14663, #13373, #12031, #22078 ) ) ;
#12930 = ORIENTED_EDGE ( 'NONE', *, *, #16338, .T. ) ;
#12931 = CYLINDRICAL_SURFACE ( 'NONE', #20270, 0.2999999999999999889 ) ;
#12932 = CARTESIAN_POINT ( 'NONE',  ( 25.37540678000427263, -63.74634676501045050, 3.799999999999999822 ) ) ;
#12933 = EDGE_CURVE ( 'NONE', #15453, #18705, #19826, .T. ) ;
#12934 = ORIENTED_EDGE ( 'NONE', *, *, #16107, .T. ) ;
#12935 = EDGE_CURVE ( 'NONE', #16682, #19790, #6051, .T. ) ;
#12936 = ORIENTED_EDGE ( 'NONE', *, *, #5532, .T. ) ;
#12937 = DIRECTION ( 'NONE',  ( -0.000000000000000000, -0.000000000000000000, -1.000000000000000000 ) ) ;
#12938 = DIRECTION ( 'NONE',  ( 0.000000000000000000, 0.000000000000000000, 1.000000000000000000 ) ) ;
#12939 = CARTESIAN_POINT ( 'NONE',  ( -23.02398829872514341, -2.245853328535781124, 13.29652846991536030 ) ) ;
#12940 = AXIS2_PLACEMENT_3D ( 'NONE', #13796, #10365, #10028 ) ;
#12941 = CARTESIAN_POINT ( 'NONE',  ( 0.000000000000000000, 71.70000000000001705, 1.500000000000000000 ) ) ;
#12942 = CARTESIAN_POINT ( 'NONE',  ( -27.37540678000427619, 5.683640910026986681, 42.50000000000000000 ) ) ;
#12943 = CARTESIAN_POINT ( 'NONE',  ( 30.07540678000427548, 0.000000000000000000, 7.500000000000000000 ) ) ;
#12944 = CARTESIAN_POINT ( 'NONE',  ( -35.00000000000001421, -84.70000000000001705, 79.70000000000000284 ) ) ;
#12945 = DIRECTION ( 'NONE',  ( 0.000000000000000000, -0.000000000000000000, -1.000000000000000000 ) ) ;
#12946 = LINE ( 'NONE', #4691, #21761 ) ;
#12947 = ORIENTED_EDGE ( 'NONE', *, *, #7630, .T. ) ;
#12948 = DIRECTION ( 'NONE',  ( -1.000000000000000000, 0.000000000000000000, 0.000000000000000000 ) ) ;
#12949 = ADVANCED_FACE ( 'NONE', ( #5577 ), #2097, .T. ) ;
#12950 = DIRECTION ( 'NONE',  ( 1.000000000000000000, 0.000000000000000000, 0.000000000000000000 ) ) ;
#12951 = DIRECTION ( 'NONE',  ( -2.546383084002652634E-16, 0.000000000000000000, -1.000000000000000000 ) ) ;
#12952 = ORIENTED_EDGE ( 'NONE', *, *, #4293, .T. ) ;
#12953 = DIRECTION ( 'NONE',  ( -0.000000000000000000, -0.000000000000000000, -1.000000000000000000 ) ) ;
#12954 = ORIENTED_EDGE ( 'NONE', *, *, #15664, .F. ) ;
#12955 = ORIENTED_EDGE ( 'NONE', *, *, #13020, .F. ) ;
#12956 = CARTESIAN_POINT ( 'NONE',  ( -33.20000000000000284, -84.70000000000001705, 1.200000000000000400 ) ) ;
#12958 = EDGE_CURVE ( 'NONE', #19724, #1963, #17556, .T. ) ;
#12957 = CONTEXT_DEPENDENT_SHAPE_REPRESENTATION ( #20734, #4455 ) ;
#12959 = ORIENTED_EDGE ( 'NONE', *, *, #15403, .F. ) ;
#12960 = ORIENTED_EDGE ( 'NONE', *, *, #11066, .F. ) ;
#12961 = FACE_OUTER_BOUND ( 'NONE', #3605, .T. ) ;
#12962 = DIRECTION ( 'NONE',  ( 1.224646799147353207E-16, 1.000000000000000000, 0.000000000000000000 ) ) ;
#12963 = VERTEX_POINT ( 'NONE', #14158 ) ;
#12964 = DIRECTION ( 'NONE',  ( 0.000000000000000000, 0.000000000000000000, 1.000000000000000000 ) ) ;
#12965 = FACE_OUTER_BOUND ( 'NONE', #20758, .T. ) ;
#12966 = DIRECTION ( 'NONE',  ( 0.000000000000000000, 0.000000000000000000, 1.000000000000000000 ) ) ;
#12967 = CARTESIAN_POINT ( 'NONE',  ( -3.627054932750481964, -32.93424481021354921, 13.50000000000000000 ) ) ;
#12968 = CARTESIAN_POINT ( 'NONE',  ( 1.724728116533979838, 42.31054587065082728, 45.66679706732590205 ) ) ;
#12969 = EDGE_CURVE ( 'NONE', #12793, #16058, #15799, .T. ) ;
#12970 = CARTESIAN_POINT ( 'NONE',  ( -34.39999999999999858, 85.00000000000000000, 0.6000000000000033085 ) ) ;
#12971 = SPHERICAL_SURFACE ( 'NONE', #6174, 0.2999999999999999889 ) ;
#12972 = EDGE_CURVE ( 'NONE', #1711, #2078, #11102, .T. ) ;
#12973 = DIRECTION ( 'NONE',  ( 0.000000000000000000, -1.000000000000000000, -0.000000000000000000 ) ) ;
#12974 = ORIENTED_EDGE ( 'NONE', *, *, #640, .F. ) ;
#12975 = DIRECTION ( 'NONE',  ( 0.000000000000000000, -0.000000000000000000, -1.000000000000000000 ) ) ;
#12976 = DIRECTION ( 'NONE',  ( 1.000000000000000000, 0.000000000000000000, 0.000000000000000000 ) ) ;
#12977 = VERTEX_POINT ( 'NONE', #9586 ) ;
#12978 = EDGE_LOOP ( 'NONE', ( #13850, #21745, #19743, #19063 ) ) ;
#12979 = DIRECTION ( 'NONE',  ( 1.000000000000000000, -0.000000000000000000, 6.123233995736764803E-17 ) ) ;
#12980 = FILL_AREA_STYLE ('',( #11758 ) ) ;
#12981 = VERTEX_POINT ( 'NONE', #16265 ) ;
#12982 = CARTESIAN_POINT ( 'NONE',  ( 27.37540678000427619, 5.683640910026986681, 13.79999999999999893 ) ) ;
#12983 = AXIS2_PLACEMENT_3D ( 'NONE', #9136, #3772, #8714 ) ;
#12984 = EDGE_CURVE ( 'NONE', #3099, #18098, #14716, .T. ) ;
#12985 = ORIENTED_EDGE ( 'NONE', *, *, #504, .F. ) ;
#12986 = CARTESIAN_POINT ( 'NONE',  ( 25.37540678000427263, -63.74634676501045050, 13.19999999999999929 ) ) ;
#12987 = PRODUCT_DEFINITION_FORMATION_WITH_SPECIFIED_SOURCE ( 'ANY', '', #20392, .NOT_KNOWN. ) ;
#12988 = LINE ( 'NONE', #18031, #17710 ) ;
#12989 = TOROIDAL_SURFACE ( 'NONE', #20533, 4.700000000000004619, 0.2999999999999999889 ) ;
#12990 = VERTEX_POINT ( 'NONE', #949 ) ;
#12991 = SURFACE_STYLE_FILL_AREA ( #21306 ) ;
#12992 = ADVANCED_FACE ( 'NONE', ( #9460 ), #13148, .T. ) ;
#12993 = DIRECTION ( 'NONE',  ( 0.000000000000000000, 0.000000000000000000, 1.000000000000000000 ) ) ;
#12994 = DIRECTION ( 'NONE',  ( 0.000000000000000000, 0.000000000000000000, 1.000000000000000000 ) ) ;
#12995 = DIRECTION ( 'NONE',  ( 0.000000000000000000, 0.000000000000000000, 1.000000000000000000 ) ) ;
#12996 = VERTEX_POINT ( 'NONE', #21789 ) ;
#12997 = DIRECTION ( 'NONE',  ( 1.000000000000000000, 0.000000000000000000, 0.000000000000000000 ) ) ;
#12998 = DIRECTION ( 'NONE',  ( 0.000000000000000000, -1.000000000000000000, 0.000000000000000000 ) ) ;
#12999 = VERTEX_POINT ( 'NONE', #6130 ) ;
#13000 = ORIENTED_EDGE ( 'NONE', *, *, #3210, .F. ) ;
#13001 = ORIENTED_EDGE ( 'NONE', *, *, #12229, .T. ) ;
#13002 = DIRECTION ( 'NONE',  ( 1.000000000000000000, -0.000000000000000000, -0.000000000000000000 ) ) ;
#13003 = EDGE_LOOP ( 'NONE', ( #2840, #14807, #17898, #8750 ) ) ;
#13004 = DIRECTION ( 'NONE',  ( -0.000000000000000000, -0.000000000000000000, -1.000000000000000000 ) ) ;
#13005 = VECTOR ( 'NONE', #9195, 1000.000000000000000 ) ;
#13006 = ADVANCED_FACE ( 'NONE', ( #16601 ), #1394, .F. ) ;
#13007 = EDGE_LOOP ( 'NONE', ( #3804, #19858, #21913, #20850 ) ) ;
#13008 = DIRECTION ( 'NONE',  ( 1.000000000000000000, 0.000000000000000000, 0.000000000000000000 ) ) ;
#13009 = CARTESIAN_POINT ( 'NONE',  ( -1.724728116533986721, 42.36054587065083155, 51.75876104995654003 ) ) ;
#13010 = DIRECTION ( 'NONE',  ( -0.000000000000000000, 0.000000000000000000, 1.000000000000000000 ) ) ;
#13011 = DIRECTION ( 'NONE',  ( 0.000000000000000000, 1.000000000000000000, 0.000000000000000000 ) ) ;
#13012 = DIRECTION ( 'NONE',  ( -0.000000000000000000, 1.000000000000000000, 0.000000000000000000 ) ) ;
#13013 = CARTESIAN_POINT ( 'NONE',  ( 29.37540678000427619, -6.000000000000000000, 7.500000000000000000 ) ) ;
#13014 = ORIENTED_EDGE ( 'NONE', *, *, #14136, .T. ) ;
#13015 = DIRECTION ( 'NONE',  ( -0.000000000000000000, -1.000000000000000000, -0.000000000000000000 ) ) ;
#13016 = DIRECTION ( 'NONE',  ( 0.000000000000000000, 0.000000000000000000, -1.000000000000000000 ) ) ;
#13017 = EDGE_CURVE ( 'NONE', #6925, #10275, #7807, .T. ) ;
#13018 = EDGE_CURVE ( 'NONE', #17187, #8250, #19876, .T. ) ;
#13019 = CARTESIAN_POINT ( 'NONE',  ( -1.824728116533986810, 42.36054587065083155, 29.66679706732590560 ) ) ;
#13020 = EDGE_CURVE ( 'NONE', #16312, #2663, #14606, .T. ) ;
#13021 = LINE ( 'NONE', #18191, #9078 ) ;
#13022 = CARTESIAN_POINT ( 'NONE',  ( -23.32398829872514057, 3.528912754968630328, 13.79999999999999893 ) ) ;
#13023 = ORIENTED_EDGE ( 'NONE', *, *, #19626, .T. ) ;
#13024 = DIRECTION ( 'NONE',  ( 1.000000000000000000, 0.000000000000000000, 0.000000000000000000 ) ) ;
#13025 = VECTOR ( 'NONE', #9041, 1000.000000000000000 ) ;
#13026 = LINE ( 'NONE', #1279, #2528 ) ;
#13027 = ORIENTED_EDGE ( 'NONE', *, *, #14543, .T. ) ;
#13028 = DIRECTION ( 'NONE',  ( 0.000000000000000000, 0.000000000000000000, -1.000000000000000000 ) ) ;
#13029 = FACE_OUTER_BOUND ( 'NONE', #10007, .T. ) ;
#13030 = ORIENTED_EDGE ( 'NONE', *, *, #6948, .T. ) ;
#13031 = ORIENTED_EDGE ( 'NONE', *, *, #6402, .T. ) ;
#13032 = ORIENTED_EDGE ( 'NONE', *, *, #11877, .F. ) ;
#13033 = DIRECTION ( 'NONE',  ( 0.000000000000000000, -1.000000000000000000, 0.000000000000000000 ) ) ;
#13034 = DIRECTION ( 'NONE',  ( 1.000000000000000000, 0.000000000000000000, 0.000000000000000000 ) ) ;
#13035 = PLANE ( 'NONE',  #988 ) ;
#13036 = VERTEX_POINT ( 'NONE', #8239 ) ;
#13037 = VECTOR ( 'NONE', #1196, 1000.000000000000000 ) ;
#13038 = ADVANCED_FACE ( 'NONE', ( #1169 ), #6236, .F. ) ;
#13039 = ORIENTED_EDGE ( 'NONE', *, *, #18160, .F. ) ;
#13040 = DIRECTION ( 'NONE',  ( 0.000000000000000000, -1.000000000000000000, 0.000000000000000000 ) ) ;
#13041 = AXIS2_PLACEMENT_3D ( 'NONE', #16406, #6243, #13028 ) ;
#13042 = CIRCLE ( 'NONE', #22019, 0.2999999999999999334 ) ;
#13043 = LINE ( 'NONE', #6258, #5649 ) ;
#13044 = CARTESIAN_POINT ( 'NONE',  ( -28.57540678000427548, 0.000000000000000000, 13.19999999999999929 ) ) ;
#13045 = DIRECTION ( 'NONE',  ( -8.673617379884034239E-17, 0.000000000000000000, 1.000000000000000000 ) ) ;
#13046 = CARTESIAN_POINT ( 'NONE',  ( -34.40000000000001279, 84.70000000000001705, 80.00000000000000000 ) ) ;
#13047 = CARTESIAN_POINT ( 'NONE',  ( -14.71174975910705029, 32.10873716947361345, 13.75000000000000000 ) ) ;
#13048 = CARTESIAN_POINT ( 'NONE',  ( -31.69597781366222122, 58.69165929845684815, 68.75000000000000000 ) ) ;
#13049 = ADVANCED_FACE ( 'NONE', ( #15051 ), #12920, .T. ) ;
#13050 = EDGE_CURVE ( 'NONE', #4630, #20393, #12216, .T. ) ;
#13051 = CARTESIAN_POINT ( 'NONE',  ( 0.000000000000000000, 5.000000000000000000, 3.799999999999999822 ) ) ;
#13052 = DIRECTION ( 'NONE',  ( 0.000000000000000000, 0.000000000000000000, 1.000000000000000000 ) ) ;
#13053 = ORIENTED_EDGE ( 'NONE', *, *, #1624, .F. ) ;
#13054 = DIRECTION ( 'NONE',  ( 1.000000000000000000, 0.000000000000000000, 0.000000000000000000 ) ) ;
#13055 = VECTOR ( 'NONE', #14424, 1000.000000000000000 ) ;
#13056 = EDGE_CURVE ( 'NONE', #14159, #4394, #11160, .T. ) ;
#13057 = DIRECTION ( 'NONE',  ( 0.000000000000000000, 0.000000000000000000, 1.000000000000000000 ) ) ;
#13058 = DIRECTION ( 'NONE',  ( 1.000000000000000000, 0.000000000000000000, 0.000000000000000000 ) ) ;
#13059 = VERTEX_POINT ( 'NONE', #4429 ) ;
#13060 = VECTOR ( 'NONE', #12629, 1000.000000000000000 ) ;
#13061 = VECTOR ( 'NONE', #3977, 1000.000000000000000 ) ;
#13062 = VECTOR ( 'NONE', #12678, 1000.000000000000000 ) ;
#13063 = DIRECTION ( 'NONE',  ( 0.8949343913984425525, 3.124646727056599230E-15, 0.4461977533474359991 ) ) ;
#13064 = DIRECTION ( 'NONE',  ( -4.336808689941893885E-15, 0.000000000000000000, 1.000000000000000000 ) ) ;
#13065 = ORIENTED_EDGE ( 'NONE', *, *, #9720, .F. ) ;
#13066 = ORIENTED_EDGE ( 'NONE', *, *, #925, .T. ) ;
#13067 = CARTESIAN_POINT ( 'NONE',  ( -1.774728116533986766, 42.36054587065083155, 35.70876104995653577 ) ) ;
#13068 = ADVANCED_FACE ( 'NONE', ( #2748 ), #7917, .F. ) ;
#13069 = ORIENTED_EDGE ( 'NONE', *, *, #10048, .T. ) ;
#13070 = AXIS2_PLACEMENT_3D ( 'NONE', #15552, #17582, #4049 ) ;
#13071 = CIRCLE ( 'NONE', #19159, 0.2500000000000002220 ) ;
#13072 = VECTOR ( 'NONE', #7735, 1000.000000000000000 ) ;
#13073 = EDGE_CURVE ( 'NONE', #17862, #6754, #10773, .T. ) ;
#13074 = DIRECTION ( 'NONE',  ( 1.095978537872987245E-16, -0.4461977533474357216, 0.8949343913984425525 ) ) ;
#13075 = DIRECTION ( 'NONE',  ( 1.734723475976806848E-16, 0.000000000000000000, -1.000000000000000000 ) ) ;
#13076 = AXIS2_PLACEMENT_3D ( 'NONE', #12220, #15695, #2047 ) ;
#13077 = DIRECTION ( 'NONE',  ( 0.000000000000000000, 0.000000000000000000, 1.000000000000000000 ) ) ;
#13078 = DIRECTION ( 'NONE',  ( -0.000000000000000000, 1.000000000000000000, -0.000000000000000000 ) ) ;
#13079 = DIRECTION ( 'NONE',  ( 0.000000000000000000, 0.000000000000000000, 1.000000000000000000 ) ) ;
#13080 = DIRECTION ( 'NONE',  ( 0.000000000000000000, 1.000000000000000000, 0.000000000000000000 ) ) ;
#13081 = DIRECTION ( 'NONE',  ( 0.000000000000000000, 0.000000000000000000, -1.000000000000000000 ) ) ;
#13082 = ADVANCED_FACE ( 'NONE', ( #18192 ), #10106, .T. ) ;
#13083 = CARTESIAN_POINT ( 'NONE',  ( -30.49999999999998934, 70.00000000000000000, 1.199999999999999512 ) ) ;
#13084 = CARTESIAN_POINT ( 'NONE',  ( 9.178906393579156386, 42.46645089659917716, 70.50000000000000000 ) ) ;
#13085 = AXIS2_PLACEMENT_3D ( 'NONE', #21662, #11230, #14594 ) ;
#13086 = DIRECTION ( 'NONE',  ( 1.000000000000000000, 0.000000000000000000, 0.000000000000000000 ) ) ;
#13087 = AXIS2_PLACEMENT_3D ( 'NONE', #8126, #8236, #12916 ) ;
#13088 = AXIS2_PLACEMENT_3D ( 'NONE', #1619, #1285, #10138 ) ;
#13089 = TOROIDAL_SURFACE ( 'NONE', #9160, 0.05000000000000000278, 0.05000000000000000278 ) ;
#13090 = ORIENTED_EDGE ( 'NONE', *, *, #21972, .T. ) ;
#13091 = FACE_OUTER_BOUND ( 'NONE', #8646, .T. ) ;
#13092 = FACE_OUTER_BOUND ( 'NONE', #895, .T. ) ;
#13093 = ORIENTED_EDGE ( 'NONE', *, *, #13103, .T. ) ;
#13094 = AXIS2_PLACEMENT_3D ( 'NONE', #1243, #14680, #6312 ) ;
#13095 = ORIENTED_EDGE ( 'NONE', *, *, #8847, .T. ) ;
#13096 = CARTESIAN_POINT ( 'NONE',  ( -29.69597781366221767, 58.69165929845684104, 70.50000000000000000 ) ) ;
#13097 = UNCERTAINTY_MEASURE_WITH_UNIT (LENGTH_MEASURE( 1.000000000000000082E-05 ), #21644, 'distance_accuracy_value', 'NONE');
#13098 = DIRECTION ( 'NONE',  ( 0.000000000000000000, 0.000000000000000000, 1.000000000000000000 ) ) ;
#13099 = EDGE_LOOP ( 'NONE', ( #6106, #19304, #2651, #21085 ) ) ;
#13100 = EDGE_CURVE ( 'NONE', #21631, #2238, #18299, .T. ) ;
#13101 = EDGE_LOOP ( 'NONE', ( #6274, #21, #21958, #9285 ) ) ;
#13102 = CIRCLE ( 'NONE', #1674, 5.000000000000004441 ) ;
#13103 = EDGE_CURVE ( 'NONE', #17419, #847, #14937, .T. ) ;
#13104 = EDGE_CURVE ( 'NONE', #20783, #2503, #16835, .T. ) ;
#13105 = TOROIDAL_SURFACE ( 'NONE', #7066, 2.800000000000002043, 0.2999999999999999889 ) ;
#13106 = VECTOR ( 'NONE', #13653, 1000.000000000000000 ) ;
#13107 = ORIENTED_EDGE ( 'NONE', *, *, #20047, .T. ) ;
#13108 = CIRCLE ( 'NONE', #15960, 0.05000000000000143219 ) ;
#13109 = CARTESIAN_POINT ( 'NONE',  ( 23.02398829872513986, 5.683640910026983128, 42.50000000000000000 ) ) ;
#13110 = VECTOR ( 'NONE', #17155, 1000.000000000000000 ) ;
#13111 = ADVANCED_BREP_SHAPE_REPRESENTATION ( '', ( #13188, #17493 ), #5511 ) ;
#13112 = CARTESIAN_POINT ( 'NONE',  ( -15.95292532278785913, -51.61873716947361856, 68.00000000000000000 ) ) ;
#13113 = CIRCLE ( 'NONE', #4910, 0.05000000000000143219 ) ;
#13114 = ORIENTED_EDGE ( 'NONE', *, *, #19201, .F. ) ;
#13115 = CARTESIAN_POINT ( 'NONE',  ( 1.724728116533979616, 42.31054587065082728, 27.80876104995653719 ) ) ;
#13116 = CARTESIAN_POINT ( 'NONE',  ( -1.724728116533986721, 43.26054587065083012, 29.66679706732590560 ) ) ;
#13117 = CARTESIAN_POINT ( 'NONE',  ( 25.37540678000427263, 63.74634676501045050, 13.50000000000000000 ) ) ;
#13118 = CARTESIAN_POINT ( 'NONE',  ( -23.04273156199907291, 2.261510999192719584, 13.21476795433022033 ) ) ;
#13119 = ORIENTED_EDGE ( 'NONE', *, *, #12099, .T. ) ;
#13120 = CYLINDRICAL_SURFACE ( 'NONE', #2187, 0.5000000000000004441 ) ;
#13121 = VECTOR ( 'NONE', #16624, 1000.000000000000000 ) ;
#13122 = EDGE_LOOP ( 'NONE', ( #2315, #2116, #5172, #17929 ) ) ;
#13123 = VECTOR ( 'NONE', #1958, 1000.000000000000000 ) ;
#13124 = VECTOR ( 'NONE', #6390, 1000.000000000000000 ) ;
#13125 = ADVANCED_FACE ( 'NONE', ( #7120 ), #20654, .T. ) ;
#13126 = ORIENTED_EDGE ( 'NONE', *, *, #5313, .F. ) ;
#13127 = ORIENTED_EDGE ( 'NONE', *, *, #20069, .T. ) ;
#13128 = DIRECTION ( 'NONE',  ( 1.000000000000000000, 0.000000000000000000, 0.000000000000000000 ) ) ;
#13129 = DIRECTION ( 'NONE',  ( -1.000000000000000000, 0.000000000000000000, 0.000000000000000000 ) ) ;
#13130 = VERTEX_POINT ( 'NONE', #6909 ) ;
#13131 = CIRCLE ( 'NONE', #12402, 0.05000000000000143219 ) ;
#13132 = DIRECTION ( 'NONE',  ( 2.107255972849994642E-16, 0.000000000000000000, 1.000000000000000000 ) ) ;
#13133 = AXIS2_PLACEMENT_3D ( 'NONE', #6892, #4854, #10008 ) ;
#13134 = EDGE_CURVE ( 'NONE', #12714, #17862, #7204, .T. ) ;
#13135 = VERTEX_POINT ( 'NONE', #12124 ) ;
#13136 = DIRECTION ( 'NONE',  ( 0.000000000000000000, 1.000000000000000000, 0.000000000000000000 ) ) ;
#13137 = EDGE_CURVE ( 'NONE', #18691, #4007, #10062, .T. ) ;
#13138 = DIRECTION ( 'NONE',  ( 1.000000000000000000, 0.000000000000000000, 0.000000000000000000 ) ) ;
#13139 = DIRECTION ( 'NONE',  ( -1.000000000000000000, 0.000000000000000000, 0.000000000000000000 ) ) ;
#13140 = AXIS2_PLACEMENT_3D ( 'NONE', #19096, #2411, #2192 ) ;
#13141 = TOROIDAL_SURFACE ( 'NONE', #9220, 0.5000000000000000000, 0.2500000000000000000 ) ;
#13142 = DIRECTION ( 'NONE',  ( 3.052134192567367925E-16, -1.000000000000000000, 0.000000000000000000 ) ) ;
#13143 = ORIENTED_EDGE ( 'NONE', *, *, #13382, .F. ) ;
#13144 = DIRECTION ( 'NONE',  ( 0.000000000000000000, 0.000000000000000000, 1.000000000000000000 ) ) ;
#13145 = DIRECTION ( 'NONE',  ( 1.000000000000000000, 0.000000000000000000, 0.000000000000000000 ) ) ;
#13146 = CIRCLE ( 'NONE', #21030, 0.5000000000000004441 ) ;
#13147 = DIRECTION ( 'NONE',  ( 0.000000000000000000, -0.000000000000000000, 1.000000000000000000 ) ) ;
#13148 = CYLINDRICAL_SURFACE ( 'NONE', #3266, 0.2499999999999985845 ) ;
#13149 = ORIENTED_EDGE ( 'NONE', *, *, #4785, .T. ) ;
#13150 = CARTESIAN_POINT ( 'NONE',  ( -30.19999999999999574, 69.70000000000001705, 2.710505431213761085E-16 ) ) ;
#13151 = VECTOR ( 'NONE', #6299, 1000.000000000000000 ) ;
#13152 = CARTESIAN_POINT ( 'NONE',  ( -15.21174975910705207, 41.81054587065082728, 68.25000000000000000 ) ) ;
#13153 = CIRCLE ( 'NONE', #9232, 0.2500000000000002220 ) ;
#13154 = ORIENTED_EDGE ( 'NONE', *, *, #66, .T. ) ;
#13155 = CARTESIAN_POINT ( 'NONE',  ( 30.79999999999999716, -123.9599366953518711, 0.3000000000000033751 ) ) ;
#13156 = CARTESIAN_POINT ( 'NONE',  ( -26.56227312273159313, 9.958410664601840878, 42.50000000000000000 ) ) ;
#13157 = EDGE_CURVE ( 'NONE', #4505, #814, #18674, .T. ) ;
#13158 = ORIENTED_EDGE ( 'NONE', *, *, #15366, .T. ) ;
#13159 = VERTEX_POINT ( 'NONE', #7006 ) ;
#13160 = ORIENTED_EDGE ( 'NONE', *, *, #4196, .T. ) ;
#13161 = CARTESIAN_POINT ( 'NONE',  ( -1.724728116533986721, 43.26054587065083012, 39.70876104995653577 ) ) ;
#13162 = DIRECTION ( 'NONE',  ( 0.000000000000000000, 0.000000000000000000, 1.000000000000000000 ) ) ;
#13163 = CARTESIAN_POINT ( 'NONE',  ( -15.21174975910705207, 41.81054587065082728, 13.50000000000000000 ) ) ;
#13164 = AXIS2_PLACEMENT_3D ( 'NONE', #20405, #16806, #1477 ) ;
#13165 = ORIENTED_EDGE ( 'NONE', *, *, #19216, .T. ) ;
#13166 = EDGE_CURVE ( 'NONE', #13756, #7310, #18622, .T. ) ;
#13167 = AXIS2_PLACEMENT_3D ( 'NONE', #13048, #14745, #11390 ) ;
#13168 = ORIENTED_EDGE ( 'NONE', *, *, #16723, .F. ) ;
#13169 = CARTESIAN_POINT ( 'NONE',  ( 1.724728116533979616, 42.31054587065082728, 51.75876104995654003 ) ) ;
#13170 = VECTOR ( 'NONE', #17596, 1000.000000000000000 ) ;
#13171 = VECTOR ( 'NONE', #18588, 1000.000000000000000 ) ;
#13172 = AXIS2_PLACEMENT_3D ( 'NONE', #21605, #13063, #12719 ) ;
#13173 = CYLINDRICAL_SURFACE ( 'NONE', #3863, 0.3000000000000016542 ) ;
#13174 = CARTESIAN_POINT ( 'NONE',  ( -23.02398829872513986, -2.191402100636986816, 13.32997043993373332 ) ) ;
#13175 = DIRECTION ( 'NONE',  ( 0.000000000000000000, 0.000000000000000000, -1.000000000000000000 ) ) ;
#13176 = DIRECTION ( 'NONE',  ( 0.000000000000000000, 0.000000000000000000, -1.000000000000000000 ) ) ;
#13177 = CARTESIAN_POINT ( 'NONE',  ( 0.000000000000000000, 5.000000000000000000, 7.500000000000000000 ) ) ;
#13178 = ORIENTED_EDGE ( 'NONE', *, *, #8296, .F. ) ;
#13179 = CARTESIAN_POINT ( 'NONE',  ( 1.724728116533979838, 42.36054587065083155, 37.66679706732590915 ) ) ;
#13180 = FACE_OUTER_BOUND ( 'NONE', #11894, .T. ) ;
#13181 = CARTESIAN_POINT ( 'NONE',  ( -21.92816239687475743, 42.46645089659918426, 68.25000000000000000 ) ) ;
#13182 = VERTEX_POINT ( 'NONE', #1847 ) ;
#13183 = CIRCLE ( 'NONE', #14239, 0.3000000000000016542 ) ;
#13184 = DIRECTION ( 'NONE',  ( 0.000000000000000000, 1.000000000000000000, 0.000000000000000000 ) ) ;
#13185 = EDGE_CURVE ( 'NONE', #12411, #11808, #3309, .T. ) ;
#13186 = AXIS2_PLACEMENT_3D ( 'NONE', #2745, #729, #835 ) ;
#13187 = CARTESIAN_POINT ( 'NONE',  ( -9.718906393579157310, 41.43704565779017202, 70.88527860057354246 ) ) ;
#13188 = MANIFOLD_SOLID_BREP ( 'Stock-MAS-696-1', #1321 ) ;
#13189 = EDGE_LOOP ( 'NONE', ( #14185, #1017, #11788, #14081 ) ) ;
#13190 = CARTESIAN_POINT ( 'NONE',  ( -3.127054932750481964, -32.61873716947361856, 68.50000000000000000 ) ) ;
#13191 = ORIENTED_EDGE ( 'NONE', *, *, #16045, .T. ) ;
#13192 = ORIENTED_EDGE ( 'NONE', *, *, #8509, .T. ) ;
#13193 = CARTESIAN_POINT ( 'NONE',  ( 26.37540678000427619, -10.94079601157914716, 13.79999999999999893 ) ) ;
#13194 = ADVANCED_FACE ( 'NONE', ( #22124 ), #8781, .T. ) ;
#13195 = EDGE_CURVE ( 'NONE', #3729, #4334, #3201, .T. ) ;
#13196 = ADVANCED_FACE ( 'NONE', ( #4990 ), #8982, .T. ) ;
#13197 = VERTEX_POINT ( 'NONE', #17060 ) ;
#13198 = EDGE_CURVE ( 'NONE', #19361, #18032, #13595, .T. ) ;
#13199 = DIRECTION ( 'NONE',  ( -1.000000000000000000, 0.000000000000000000, 2.107255972849994642E-16 ) ) ;
#13200 = DIRECTION ( 'NONE',  ( -6.123233995736764803E-17, 0.000000000000000000, 1.000000000000000000 ) ) ;
#13201 = AXIS2_PLACEMENT_3D ( 'NONE', #2877, #14609, #21463 ) ;
#13202 = AXIS2_PLACEMENT_3D ( 'NONE', #3927, #19247, #17657 ) ;
#13203 = DIRECTION ( 'NONE',  ( 1.000000000000000000, 0.000000000000000000, 0.000000000000000000 ) ) ;
#13204 = LINE ( 'NONE', #16547, #4885 ) ;
#13205 = DIRECTION ( 'NONE',  ( -0.000000000000000000, 0.000000000000000000, -1.000000000000000000 ) ) ;
#13206 = CARTESIAN_POINT ( 'NONE',  ( -8.641460742840918030, -33.43424481021354921, 13.50000000000000000 ) ) ;
#13207 = ADVANCED_FACE ( 'NONE', ( #3412 ), #1738, .F. ) ;
#13208 = CARTESIAN_POINT ( 'NONE',  ( -3.127054932750481964, 32.61873716947361856, 68.00000000000000000 ) ) ;
#13209 = CARTESIAN_POINT ( 'NONE',  ( -27.37540678000427974, -10.94079601157914716, 42.50000000000000000 ) ) ;
#13210 = CARTESIAN_POINT ( 'NONE',  ( 29.09616827897941249, -6.500357068115323322, 7.499999999998635758 ) ) ;
#13211 = DIRECTION ( 'NONE',  ( -0.000000000000000000, -0.000000000000000000, -1.000000000000000000 ) ) ;
#13212 = ORIENTED_EDGE ( 'NONE', *, *, #17436, .T. ) ;
#13213 = CARTESIAN_POINT ( 'NONE',  ( -0.000000000000000000, 69.00000000000000000, 1.500000000000000000 ) ) ;
#13214 = TOROIDAL_SURFACE ( 'NONE', #1407, 0.05000000000000000278, 0.05000000000000000278 ) ;
#13215 = AXIS2_PLACEMENT_3D ( 'NONE', #16021, #7652, #10681 ) ;
#13216 = AXIS2_PLACEMENT_3D ( 'NONE', #18533, #8355, #22012 ) ;
#13217 = CARTESIAN_POINT ( 'NONE',  ( -1.824728116533986810, 43.26054587065083012, 27.80876104995653719 ) ) ;
#13218 = ORIENTED_EDGE ( 'NONE', *, *, #6661, .F. ) ;
#13219 = ORIENTED_EDGE ( 'NONE', *, *, #198, .T. ) ;
#13220 = DIRECTION ( 'NONE',  ( 2.107255972849994642E-16, -0.000000000000000000, 1.000000000000000000 ) ) ;
#13221 = EDGE_LOOP ( 'NONE', ( #20307, #9528, #17338, #3237, #5166 ) ) ;
#13222 = EDGE_CURVE ( 'NONE', #6030, #8329, #5919, .T. ) ;
#13223 = CARTESIAN_POINT ( 'NONE',  ( 1.724728116533979616, 42.31054587065082728, 45.71679706732590631 ) ) ;
#13224 = ORIENTED_EDGE ( 'NONE', *, *, #16173, .F. ) ;
#13225 = EDGE_CURVE ( 'NONE', #9395, #5807, #16478, .T. ) ;
#13226 = VERTEX_POINT ( 'NONE', #3743 ) ;
#13227 = ORIENTED_EDGE ( 'NONE', *, *, #14701, .F. ) ;
#13228 = CIRCLE ( 'NONE', #20040, 0.2999999999999999334 ) ;
#13229 = CARTESIAN_POINT ( 'NONE',  ( 14.98586301832698808, -51.95135570414442583, 13.85537332152988554 ) ) ;
#13230 = AXIS2_PLACEMENT_3D ( 'NONE', #5539, #21096, #12651 ) ;
#13231 = DIRECTION ( 'NONE',  ( -0.000000000000000000, -0.000000000000000000, -1.000000000000000000 ) ) ;
#13232 = ORIENTED_EDGE ( 'NONE', *, *, #14927, .F. ) ;
#13233 = LINE ( 'NONE', #16363, #10016 ) ;
#13234 = FACE_OUTER_BOUND ( 'NONE', #9040, .T. ) ;
#13235 = CARTESIAN_POINT ( 'NONE',  ( -32.23382792203229741, 83.71979900898287497, 13.75000000000000000 ) ) ;
#13236 = EDGE_CURVE ( 'NONE', #20218, #4038, #14740, .T. ) ;
#13237 = DIRECTION ( 'NONE',  ( -0.000000000000000000, 0.000000000000000000, -1.000000000000000000 ) ) ;
#13238 = VERTEX_POINT ( 'NONE', #17706 ) ;
#13239 = VERTEX_POINT ( 'NONE', #9106 ) ;
#13240 = ORIENTED_EDGE ( 'NONE', *, *, #1858, .T. ) ;
#13241 = CARTESIAN_POINT ( 'NONE',  ( -23.04273156199908357, 2.261510999192738680, 13.50000000000000000 ) ) ;
#13242 = AXIS2_PLACEMENT_3D ( 'NONE', #4054, #17589, #21405 ) ;
#13243 = CARTESIAN_POINT ( 'NONE',  ( -29.13662752439705272, 0.000000000000000000, 3.799999999999999822 ) ) ;
#13244 = ORIENTED_EDGE ( 'NONE', *, *, #21073, .T. ) ;
#13245 = AXIS2_PLACEMENT_3D ( 'NONE', #7414, #21074, #12530 ) ;
#13246 = DIRECTION ( 'NONE',  ( 1.000000000000000000, 0.000000000000000000, 0.000000000000000000 ) ) ;
#13247 = EDGE_CURVE ( 'NONE', #15670, #21768, #21902, .T. ) ;
#13248 = ORIENTED_EDGE ( 'NONE', *, *, #2659, .F. ) ;
#13249 = DIRECTION ( 'NONE',  ( 0.000000000000000000, -1.000000000000000000, 0.000000000000000000 ) ) ;
#13250 = CARTESIAN_POINT ( 'NONE',  ( -14.96174975910705207, 51.61873716947361856, 14.00000000000000000 ) ) ;
#13251 = CARTESIAN_POINT ( 'NONE',  ( 23.02398829872513986, -2.157133568460768203, 13.26806292639400908 ) ) ;
#13252 = CARTESIAN_POINT ( 'NONE',  ( 15.95292532278785913, 52.39333383871510108, 13.79999999999999716 ) ) ;
#13253 = VERTEX_POINT ( 'NONE', #589 ) ;
#13254 = DIRECTION ( 'NONE',  ( 0.000000000000000000, -0.000000000000000000, -1.000000000000000000 ) ) ;
#13255 = CARTESIAN_POINT ( 'NONE',  ( 27.37540678000426908, 36.74634676501047181, 13.79999999999999893 ) ) ;
#13256 = AXIS2_PLACEMENT_3D ( 'NONE', #1338, #8295, #18347 ) ;
#13257 = DIRECTION ( 'NONE',  ( 1.000000000000000000, 0.000000000000000000, 0.000000000000000000 ) ) ;
#13258 = DIRECTION ( 'NONE',  ( 1.224646799147353207E-16, 0.000000000000000000, 1.000000000000000000 ) ) ;
#13259 = VERTEX_POINT ( 'NONE', #2386 ) ;
#13260 = DIRECTION ( 'NONE',  ( 1.000000000000000000, 0.000000000000000000, 0.000000000000000000 ) ) ;
#13261 = EDGE_CURVE ( 'NONE', #15983, #6525, #5110, .T. ) ;
#13262 = ORIENTED_EDGE ( 'NONE', *, *, #10143, .T. ) ;
#13263 = DIRECTION ( 'NONE',  ( 1.000000000000000000, 0.000000000000000000, 0.000000000000000000 ) ) ;
#13264 = VECTOR ( 'NONE', #13794, 1000.000000000000000 ) ;
#13265 = CARTESIAN_POINT ( 'NONE',  ( -17.95292532278785913, 0.000000000000000000, 13.99999999999999822 ) ) ;
#13266 = ADVANCED_FACE ( 'NONE', ( #16025 ), #12450, .T. ) ;
#13267 = EDGE_LOOP ( 'NONE', ( #21682, #1288, #7751, #11423 ) ) ;
#13268 = AXIS2_PLACEMENT_3D ( 'NONE', #2223, #5496, #7504 ) ;
#13269 = ORIENTED_EDGE ( 'NONE', *, *, #5423, .T. ) ;
#13270 = ORIENTED_EDGE ( 'NONE', *, *, #6644, .F. ) ;
#13271 = CARTESIAN_POINT ( 'NONE',  ( 30.79999999999999716, -84.70000000000001705, 1.500000000000004219 ) ) ;
#13272 = TOROIDAL_SURFACE ( 'NONE', #12906, 0.05000000000000000278, 0.05000000000000000278 ) ;
#13273 = DIRECTION ( 'NONE',  ( 1.000000000000000000, 0.000000000000000000, 0.000000000000000000 ) ) ;
#13274 = VECTOR ( 'NONE', #19278, 1000.000000000000000 ) ;
#13275 = EDGE_LOOP ( 'NONE', ( #13491, #5790, #11325, #4688 ) ) ;
#13276 = VERTEX_POINT ( 'NONE', #704 ) ;
#13277 = CYLINDRICAL_SURFACE ( 'NONE', #5776, 0.2500000000000002220 ) ;
#13278 = DIRECTION ( 'NONE',  ( 1.000000000000000000, -0.000000000000000000, -0.000000000000000000 ) ) ;
#13279 = DIRECTION ( 'NONE',  ( 0.000000000000000000, 0.000000000000000000, -1.000000000000000000 ) ) ;
#13280 = DIRECTION ( 'NONE',  ( 0.000000000000000000, 0.000000000000000000, 1.000000000000000000 ) ) ;
#13281 = ADVANCED_FACE ( 'NONE', ( #5873 ), #19299, .F. ) ;
#13282 = CIRCLE ( 'NONE', #15074, 0.2999999999999999334 ) ;
#13283 = LINE ( 'NONE', #4790, #12136 ) ;
#13284 = DIRECTION ( 'NONE',  ( 0.000000000000000000, 0.000000000000000000, -1.000000000000000000 ) ) ;
#13285 = ORIENTED_EDGE ( 'NONE', *, *, #12126, .F. ) ;
#13286 = DIRECTION ( 'NONE',  ( -0.000000000000000000, -1.000000000000000000, 0.000000000000000000 ) ) ;
#13287 = AXIS2_PLACEMENT_3D ( 'NONE', #19600, #2480, #9647 ) ;
#13288 = CIRCLE ( 'NONE', #4725, 2.000000000000001776 ) ;
#13289 = AXIS2_PLACEMENT_3D ( 'NONE', #14002, #14100, #7205 ) ;
#13290 = CARTESIAN_POINT ( 'NONE',  ( -35.00000000000000000, 85.00000000000000000, 0.6000000000000033085 ) ) ;
#13291 = ORIENTED_EDGE ( 'NONE', *, *, #854, .F. ) ;
#13292 = FACE_OUTER_BOUND ( 'NONE', #17416, .T. ) ;
#13293 = CIRCLE ( 'NONE', #6535, 2.767785046117004377 ) ;
#13294 = ADVANCED_FACE ( 'NONE', ( #374 ), #7441, .T. ) ;
#13295 = EDGE_CURVE ( 'NONE', #8916, #7627, #2167, .T. ) ;
#13296 = ORIENTED_EDGE ( 'NONE', *, *, #21843, .T. ) ;
#13297 = DIRECTION ( 'NONE',  ( 0.000000000000000000, 0.000000000000000000, 1.000000000000000000 ) ) ;
#13298 = DIRECTION ( 'NONE',  ( 0.000000000000000000, 0.000000000000000000, -1.000000000000000000 ) ) ;
#13299 = ORIENTED_EDGE ( 'NONE', *, *, #7197, .F. ) ;
#13300 = ORIENTED_EDGE ( 'NONE', *, *, #1491, .F. ) ;
#13301 = CARTESIAN_POINT ( 'NONE',  ( 29.42156510615627596, -2.562837254968982403, 0.09431619747333748471 ) ) ;
#13302 = AXIS2_PLACEMENT_3D ( 'NONE', #18228, #7616, #21159 ) ;
#13303 = ORIENTED_EDGE ( 'NONE', *, *, #14220, .T. ) ;
#13304 = ADVANCED_FACE ( 'NONE', ( #7553 ), #3976, .F. ) ;
#13305 = CARTESIAN_POINT ( 'NONE',  ( 29.20000000000002061, 0.000000000000000000, 0.2999999999999947153 ) ) ;
#13306 = ORIENTED_EDGE ( 'NONE', *, *, #17785, .T. ) ;
#13307 = DIRECTION ( 'NONE',  ( 1.000000000000000000, 0.000000000000000000, 0.000000000000000000 ) ) ;
#13308 = AXIS2_PLACEMENT_3D ( 'NONE', #6649, #3174, #6769 ) ;
#13309 = FACE_OUTER_BOUND ( 'NONE', #3882, .T. ) ;
#13310 = CARTESIAN_POINT ( 'NONE',  ( 17.95292532278785913, 0.000000000000000000, 42.50000000000000711 ) ) ;
#13311 = DIRECTION ( 'NONE',  ( -0.000000000000000000, 0.000000000000000000, 1.000000000000000000 ) ) ;
#13312 = CARTESIAN_POINT ( 'NONE',  ( 0.000000000000000000, 42.31054587065082728, 45.71679706732590631 ) ) ;
#13313 = ADVANCED_FACE ( 'NONE', ( #12655 ), #10686, .T. ) ;
#13314 = ADVANCED_FACE ( 'NONE', ( #2500 ), #1837, .T. ) ;
#13315 = DIRECTION ( 'NONE',  ( -1.000000000000000000, -0.000000000000000000, 0.000000000000000000 ) ) ;
#13316 = EDGE_CURVE ( 'NONE', #12280, #8060, #20450, .T. ) ;
#13317 = FACE_OUTER_BOUND ( 'NONE', #2009, .T. ) ;
#13318 = LINE ( 'NONE', #8397, #15867 ) ;
#13319 = PLANE ( 'NONE',  #17390 ) ;
#13320 = ORIENTED_EDGE ( 'NONE', *, *, #12503, .F. ) ;
#13321 = LINE ( 'NONE', #4823, #15602 ) ;
#13322 = CARTESIAN_POINT ( 'NONE',  ( -31.50000000000002132, -71.00000000000001421, 3.200000000000000178 ) ) ;
#13323 = ORIENTED_EDGE ( 'NONE', *, *, #15798, .T. ) ;
#13324 = ORIENTED_EDGE ( 'NONE', *, *, #18649, .F. ) ;
#13325 = FACE_OUTER_BOUND ( 'NONE', #7317, .T. ) ;
#13326 = VERTEX_POINT ( 'NONE', #2716 ) ;
#13327 = EDGE_CURVE ( 'NONE', #15418, #7129, #17205, .T. ) ;
#13328 = VERTEX_POINT ( 'NONE', #14449 ) ;
#13329 = ORIENTED_EDGE ( 'NONE', *, *, #5750, .T. ) ;
#13330 = CARTESIAN_POINT ( 'NONE',  ( 0.000000000000000000, -39.04634676501046187, 13.79999999999999893 ) ) ;
#13331 = CARTESIAN_POINT ( 'NONE',  ( 0.000000000000000000, 32.11873716947361856, 109.6002446535588319 ) ) ;
#13332 = ORIENTED_EDGE ( 'NONE', *, *, #13453, .F. ) ;
#13333 = CARTESIAN_POINT ( 'NONE',  ( 29.37540678000427619, 6.000000000000000000, 7.200000000000000178 ) ) ;
#13334 = EDGE_CURVE ( 'NONE', #3057, #21013, #15421, .T. ) ;
#13335 = DIRECTION ( 'NONE',  ( 0.000000000000000000, 1.000000000000000000, -0.000000000000000000 ) ) ;
#13336 = EDGE_CURVE ( 'NONE', #16692, #10531, #10784, .T. ) ;
#13337 = DIRECTION ( 'NONE',  ( 0.000000000000000000, 0.000000000000000000, 1.000000000000000000 ) ) ;
#13338 = AXIS2_PLACEMENT_3D ( 'NONE', #16678, #14669, #7980 ) ;
#13339 = CARTESIAN_POINT ( 'NONE',  ( 33.19999999999999574, -85.00000000000000000, 1.200000000000004396 ) ) ;
#13340 = EDGE_CURVE ( 'NONE', #11153, #14847, #5788, .T. ) ;
#13341 = LINE ( 'NONE', #16239, #17912 ) ;
#13342 = ORIENTED_EDGE ( 'NONE', *, *, #4528, .T. ) ;
#13343 = ORIENTED_EDGE ( 'NONE', *, *, #3606, .F. ) ;
#13344 = ORIENTED_EDGE ( 'NONE', *, *, #9675, .T. ) ;
#13345 = CARTESIAN_POINT ( 'NONE',  ( 9.178906393579156386, 42.46645089659917716, 70.50000000000000000 ) ) ;
#13346 = DIRECTION ( 'NONE',  ( 0.000000000000000000, 0.000000000000000000, -1.000000000000000000 ) ) ;
#13347 = AXIS2_PLACEMENT_3D ( 'NONE', #4540, #7806, #2422 ) ;
#13348 = ORIENTED_EDGE ( 'NONE', *, *, #9429, .T. ) ;
#13349 = CARTESIAN_POINT ( 'NONE',  ( -1.774728116533986544, 43.31054587065082728, 47.80876104995653719 ) ) ;
#13350 = EDGE_CURVE ( 'NONE', #14858, #19370, #7991, .T. ) ;
#13351 = VECTOR ( 'NONE', #14659, 1000.000000000000000 ) ;
#13352 = ORIENTED_EDGE ( 'NONE', *, *, #15131, .T. ) ;
#13353 = AXIS2_PLACEMENT_3D ( 'NONE', #5772, #9550, #9217 ) ;
#13354 = PLANE ( 'NONE',  #1797 ) ;
#13355 = AXIS2_PLACEMENT_3D ( 'NONE', #9801, #8343, #6677 ) ;
#13356 = DIRECTION ( 'NONE',  ( 0.000000000000000000, 0.000000000000000000, 1.000000000000000000 ) ) ;
#13357 = EDGE_CURVE ( 'NONE', #18586, #18072, #8645, .T. ) ;
#13358 = DIRECTION ( 'NONE',  ( 0.000000000000000000, 1.000000000000000000, 0.000000000000000000 ) ) ;
#13359 = CARTESIAN_POINT ( 'NONE',  ( -10.73004499984425841, -2.546852060775805615, 68.25000000000000000 ) ) ;
#13360 = VERTEX_POINT ( 'NONE', #4296 ) ;
#13361 = FACE_OUTER_BOUND ( 'NONE', #18819, .T. ) ;
#13362 = CARTESIAN_POINT ( 'NONE',  ( -26.56227312273159313, -9.958410664601842655, 42.50000000000000000 ) ) ;
#13363 = FACE_OUTER_BOUND ( 'NONE', #598, .T. ) ;
#13364 = LINE ( 'NONE', #13478, #18002 ) ;
#13365 = DIRECTION ( 'NONE',  ( 1.000000000000000000, 3.358721889151030981E-15, -1.224646799147353207E-16 ) ) ;
#13366 = VERTEX_POINT ( 'NONE', #21310 ) ;
#13367 = DIRECTION ( 'NONE',  ( -0.000000000000000000, 1.000000000000000000, -0.000000000000000000 ) ) ;
#13368 = EDGE_CURVE ( 'NONE', #6358, #5647, #7770, .T. ) ;
#13369 = ORIENTED_EDGE ( 'NONE', *, *, #493, .T. ) ;
#13370 = DIRECTION ( 'NONE',  ( 1.000000000000000000, 0.000000000000000000, 0.000000000000000000 ) ) ;
#13371 = CARTESIAN_POINT ( 'NONE',  ( 1.724728116533979616, 43.26054587065083012, 33.76679706732591058 ) ) ;
#13372 = ORIENTED_EDGE ( 'NONE', *, *, #8166, .T. ) ;
#13373 = ORIENTED_EDGE ( 'NONE', *, *, #3164, .T. ) ;
#13374 = ORIENTED_EDGE ( 'NONE', *, *, #6338, .F. ) ;
#13375 = CARTESIAN_POINT ( 'NONE',  ( -15.06704456860866870, 51.94509779313090547, 13.50000000000000000 ) ) ;
#13376 = CARTESIAN_POINT ( 'NONE',  ( 17.95292532278785913, -50.11873716947361856, 109.6002446535588319 ) ) ;
#13377 = VERTEX_POINT ( 'NONE', #18274 ) ;
#13378 = FACE_OUTER_BOUND ( 'NONE', #3060, .T. ) ;
#13379 = ORIENTED_EDGE ( 'NONE', *, *, #7049, .T. ) ;
#13380 = ORIENTED_EDGE ( 'NONE', *, *, #4561, .T. ) ;
#13381 = DIRECTION ( 'NONE',  ( 1.000000000000000000, 0.000000000000000000, 0.000000000000000000 ) ) ;
#13382 = EDGE_CURVE ( 'NONE', #18442, #1357, #19716, .T. ) ;
#13383 = DIRECTION ( 'NONE',  ( -4.336808689941893885E-15, 0.000000000000000000, 1.000000000000000000 ) ) ;
#13384 = LINE ( 'NONE', #10051, #4580 ) ;
#13385 = ADVANCED_FACE ( 'NONE', ( #11215 ), #14794, .T. ) ;
#13386 = FACE_OUTER_BOUND ( 'NONE', #14256, .T. ) ;
#13387 = EDGE_CURVE ( 'NONE', #7934, #6210, #16577, .T. ) ;
#13388 = AXIS2_PLACEMENT_3D ( 'NONE', #15209, #8075, #19945 ) ;
#13389 = CARTESIAN_POINT ( 'NONE',  ( 1.724728116533979616, 42.31054587065082728, 47.80876104995653719 ) ) ;
#13390 = AXIS2_PLACEMENT_3D ( 'NONE', #20846, #11985, #20516 ) ;
#13391 = CARTESIAN_POINT ( 'NONE',  ( 14.96174975910705918, -51.61873716947361856, 14.00000000000000000 ) ) ;
#13392 = ORIENTED_EDGE ( 'NONE', *, *, #9342, .F. ) ;
#13393 = LINE ( 'NONE', #10057, #5335 ) ;
#13394 = DIRECTION ( 'NONE',  ( 1.000000000000000000, 0.000000000000000000, 0.000000000000000000 ) ) ;
#13395 = PRODUCT_DEFINITION_SHAPE ( 'NONE', 'NONE',  #22171 ) ;
#13396 = DIRECTION ( 'NONE',  ( -1.000000000000000000, 0.000000000000000000, 0.000000000000000000 ) ) ;
#13397 = ORIENTED_EDGE ( 'NONE', *, *, #2585, .F. ) ;
#13398 = DIRECTION ( 'NONE',  ( -1.000000000000000000, -0.000000000000000000, -0.000000000000000000 ) ) ;
#13399 = CARTESIAN_POINT ( 'NONE',  ( -10.22290649399595353, 43.00645089659918341, 68.06527860057354928 ) ) ;
#13400 = ORIENTED_EDGE ( 'NONE', *, *, #16946, .F. ) ;
#13401 = LINE ( 'NONE', #18779, #11734 ) ;
#13402 = DIRECTION ( 'NONE',  ( 1.000000000000000000, 0.000000000000000000, 0.000000000000000000 ) ) ;
#13403 = VERTEX_POINT ( 'NONE', #6317 ) ;
#13404 = PRODUCT_RELATED_PRODUCT_CATEGORY ( 'part', '', ( #6454 ) ) ;
#13405 = AXIS2_PLACEMENT_3D ( 'NONE', #17506, #4077, #2173 ) ;
#13406 = ORIENTED_EDGE ( 'NONE', *, *, #11637, .T. ) ;
#13407 = AXIS2_PLACEMENT_3D ( 'NONE', #16164, #4104, #7810 ) ;
#13408 = DIRECTION ( 'NONE',  ( 0.000000000000000000, 0.000000000000000000, 1.000000000000000000 ) ) ;
#13409 = ORIENTED_EDGE ( 'NONE', *, *, #20786, .F. ) ;
#13410 = EDGE_CURVE ( 'NONE', #9618, #9288, #11484, .T. ) ;
#13411 = CARTESIAN_POINT ( 'NONE',  ( -9.718906393579157310, 43.42161583426526761, 69.94509975324525897 ) ) ;
#13412 = ORIENTED_EDGE ( 'NONE', *, *, #5145, .F. ) ;
#13413 = CARTESIAN_POINT ( 'NONE',  ( -15.95292532278785913, -34.11873716947361856, 42.50000000000000711 ) ) ;
#13414 = CIRCLE ( 'NONE', #1628, 0.05000000000000143219 ) ;
#13415 = DIRECTION ( 'NONE',  ( 0.000000000000000000, 0.000000000000000000, 1.000000000000000000 ) ) ;
#13416 = CARTESIAN_POINT ( 'NONE',  ( -1.824728116533986810, 43.31054587065082728, 49.66679706732590915 ) ) ;
#13417 = CARTESIAN_POINT ( 'NONE',  ( -9.641460742840918030, -33.43424481021354921, 68.50000000000000000 ) ) ;
#13418 = CIRCLE ( 'NONE', #18419, 0.3000000000000016542 ) ;
#13419 = AXIS2_PLACEMENT_3D ( 'NONE', #7355, #13936, #10711 ) ;
#13420 = DIRECTION ( 'NONE',  ( 0.000000000000000000, -0.000000000000000000, 1.000000000000000000 ) ) ;
#13421 = CARTESIAN_POINT ( 'NONE',  ( -34.39999999999999858, 84.70000000000001705, 0.6000000000000033085 ) ) ;
#13422 = CARTESIAN_POINT ( 'NONE',  ( -15.16859876043988464, -52.00603549157913363, 13.50000000000000000 ) ) ;
#13423 = CARTESIAN_POINT ( 'NONE',  ( 0.000000000000000000, -4.700000000000000178, 3.799999999999999822 ) ) ;
#13424 = CARTESIAN_POINT ( 'NONE',  ( 3.985331397971318079, 42.46645089659917716, 70.50000000000000000 ) ) ;
#13425 = ORIENTED_EDGE ( 'NONE', *, *, #2063, .F. ) ;
#13426 = DIRECTION ( 'NONE',  ( 2.107255972849994642E-16, -0.000000000000000000, 1.000000000000000000 ) ) ;
#13427 = AXIS2_PLACEMENT_3D ( 'NONE', #12632, #6282, #4269 ) ;
#13428 = ORIENTED_EDGE ( 'NONE', *, *, #1147, .F. ) ;
#13429 = CIRCLE ( 'NONE', #9508, 0.2999999999999999334 ) ;
#13430 = EDGE_LOOP ( 'NONE', ( #4430, #16357, #1970, #9334 ) ) ;
#13431 = CARTESIAN_POINT ( 'NONE',  ( 0.000000000000000000, 0.000000000000000000, 0.000000000000000000 ) ) ;
#13432 = ORIENTED_EDGE ( 'NONE', *, *, #20197, .F. ) ;
#13433 = AXIS2_PLACEMENT_3D ( 'NONE', #19936, #4599, #12738 ) ;
#13434 = VECTOR ( 'NONE', #4175, 1000.000000000000000 ) ;
#13435 = ORIENTED_EDGE ( 'NONE', *, *, #4048, .F. ) ;
#13436 = EDGE_CURVE ( 'NONE', #17256, #20393, #17572, .T. ) ;
#13437 = VERTEX_POINT ( 'NONE', #14686 ) ;
#13438 = ADVANCED_FACE ( 'NONE', ( #21542 ), #19736, .T. ) ;
#13439 = ORIENTED_EDGE ( 'NONE', *, *, #21708, .F. ) ;
#13440 = FACE_OUTER_BOUND ( 'NONE', #13692, .T. ) ;
#13441 = CARTESIAN_POINT ( 'NONE',  ( 30.79999999999999716, -84.70000000000001705, 10.00000000000000178 ) ) ;
#13442 = AXIS2_PLACEMENT_3D ( 'NONE', #19872, #13015, #11568 ) ;
#13443 = AXIS2_PLACEMENT_3D ( 'NONE', #11801, #17071, #6805 ) ;
#13444 = DIRECTION ( 'NONE',  ( -0.000000000000000000, -1.000000000000000000, -0.000000000000000000 ) ) ;
#13445 = AXIS2_PLACEMENT_3D ( 'NONE', #10083, #11849, #6619 ) ;
#13446 = ORIENTED_EDGE ( 'NONE', *, *, #19707, .F. ) ;
#13447 = DIRECTION ( 'NONE',  ( 0.000000000000000000, 0.000000000000000000, 1.000000000000000000 ) ) ;
#13448 = EDGE_CURVE ( 'NONE', #14241, #7362, #11548, .T. ) ;
#13449 = CARTESIAN_POINT ( 'NONE',  ( 1.724728116533979616, 42.36054587065083155, 53.76679706732590347 ) ) ;
#13450 = CARTESIAN_POINT ( 'NONE',  ( -1.724728116533986721, 42.31054587065082728, 27.75876104995654003 ) ) ;
#13451 = DIRECTION ( 'NONE',  ( 1.000000000000000000, 0.000000000000000000, -0.000000000000000000 ) ) ;
#13452 = CIRCLE ( 'NONE', #939, 0.5000000000000004441 ) ;
#13453 = EDGE_CURVE ( 'NONE', #18309, #6576, #11842, .T. ) ;
#13454 = DIRECTION ( 'NONE',  ( -3.387630566026860322E-15, 1.000000000000000000, -1.333119110027185404E-17 ) ) ;
#13455 = ORIENTED_EDGE ( 'NONE', *, *, #16432, .F. ) ;
#13456 = VERTEX_POINT ( 'NONE', #1247 ) ;
#13457 = ORIENTED_EDGE ( 'NONE', *, *, #1983, .F. ) ;
#13458 = CARTESIAN_POINT ( 'NONE',  ( -14.71174975910705029, 51.61873716947361856, 13.50000000000000000 ) ) ;
#13459 = CARTESIAN_POINT ( 'NONE',  ( -15.21174975910705207, -41.81054587065082728, 68.50000000000000000 ) ) ;
#13460 = ORIENTED_EDGE ( 'NONE', *, *, #20087, .F. ) ;
#13461 = VECTOR ( 'NONE', #18708, 1000.000000000000114 ) ;
#13462 = AXIS2_PLACEMENT_3D ( 'NONE', #11675, #18180, #14707 ) ;
#13463 = AXIS2_PLACEMENT_3D ( 'NONE', #11410, #21837, #20144 ) ;
#13464 = CARTESIAN_POINT ( 'NONE',  ( -33.20000000000000284, 84.70000000000001705, 1.200000000000000400 ) ) ;
#13465 = ADVANCED_FACE ( 'NONE', ( #11328 ), #18156, .T. ) ;
#13466 = CIRCLE ( 'NONE', #11671, 0.5000000000000004441 ) ;
#13467 = ADVANCED_FACE ( 'NONE', ( #1705 ), #4843, .T. ) ;
#13468 = ORIENTED_EDGE ( 'NONE', *, *, #10981, .T. ) ;
#13469 = CARTESIAN_POINT ( 'NONE',  ( -15.21174975910705207, 41.81054587065082728, 68.50000000000000000 ) ) ;
#13470 = CARTESIAN_POINT ( 'NONE',  ( -29.69597781366221767, 56.94165929845684815, 70.25000000000000000 ) ) ;
#13471 = ADVANCED_FACE ( 'NONE', ( #18830 ), #16810, .F. ) ;
#13472 = CARTESIAN_POINT ( 'NONE',  ( -15.21174975910705207, 32.10873716947361345, 68.25000000000000000 ) ) ;
#13473 = CYLINDRICAL_SURFACE ( 'NONE', #2353, 0.2500000000000001665 ) ;
#13474 = ORIENTED_EDGE ( 'NONE', *, *, #16127, .F. ) ;
#13475 = CARTESIAN_POINT ( 'NONE',  ( -19.85144383993102934, 42.46645089659918426, 68.25000000000000000 ) ) ;
#13476 = DIRECTION ( 'NONE',  ( 0.000000000000000000, 0.000000000000000000, 1.000000000000000000 ) ) ;
#13477 = CARTESIAN_POINT ( 'NONE',  ( 14.66174975910705847, 0.000000000000000000, 13.79999999999999893 ) ) ;
#13478 = CARTESIAN_POINT ( 'NONE',  ( -33.50000000000000000, 84.70000000000001705, 1.500000000000000000 ) ) ;
#13479 =( NAMED_UNIT ( * ) PLANE_ANGLE_UNIT ( ) SI_UNIT ( $, .RADIAN. ) );
#13480 = ORIENTED_EDGE ( 'NONE', *, *, #2210, .T. ) ;
#13481 = CIRCLE ( 'NONE', #12396, 5.299999999999998934 ) ;
#13482 = VECTOR ( 'NONE', #18781, 1000.000000000000000 ) ;
#13483 = DIRECTION ( 'NONE',  ( 1.000000000000000000, 0.000000000000000000, 0.000000000000000000 ) ) ;
#13484 = ADVANCED_FACE ( 'NONE', ( #11654 ), #20175, .F. ) ;
#13485 = ORIENTED_EDGE ( 'NONE', *, *, #15703, .T. ) ;
#13486 = FACE_OUTER_BOUND ( 'NONE', #6870, .T. ) ;
#13487 = AXIS2_PLACEMENT_3D ( 'NONE', #4890, #10044, #5008 ) ;
#13488 = CARTESIAN_POINT ( 'NONE',  ( 28.57540678000427548, 0.000000000000000000, 13.19999999999999929 ) ) ;
#13489 = EDGE_LOOP ( 'NONE', ( #7484, #9665, #10136, #7515 ) ) ;
#13490 = ORIENTED_EDGE ( 'NONE', *, *, #9236, .F. ) ;
#13491 = ORIENTED_EDGE ( 'NONE', *, *, #16614, .T. ) ;
#13492 = DIRECTION ( 'NONE',  ( 0.000000000000000000, 0.000000000000000000, 1.000000000000000000 ) ) ;
#13493 = AXIS2_PLACEMENT_3D ( 'NONE', #21138, #16279, #16172 ) ;
#13494 = CARTESIAN_POINT ( 'NONE',  ( 34.69999999999999574, -84.70000000000001705, 0.6000000000000033085 ) ) ;
#13495 = ORIENTED_EDGE ( 'NONE', *, *, #15199, .T. ) ;
#13496 = EDGE_CURVE ( 'NONE', #8252, #1910, #5077, .T. ) ;
#13497 = ORIENTED_EDGE ( 'NONE', *, *, #842, .T. ) ;
#13498 = AXIS2_PLACEMENT_3D ( 'NONE', #15195, #3350, #11517 ) ;
#13499 = DIRECTION ( 'NONE',  ( 0.000000000000000000, 0.000000000000000000, 1.000000000000000000 ) ) ;
#13500 = CIRCLE ( 'NONE', #8513, 0.2999999999999999334 ) ;
#13501 = ADVANCED_FACE ( 'NONE', ( #1586 ), #13272, .T. ) ;
#13502 = EDGE_LOOP ( 'NONE', ( #12704, #6991, #16846, #12360 ) ) ;
#13503 = CARTESIAN_POINT ( 'NONE',  ( -35.00000000000001421, 85.00000000000000000, 79.39999999999999147 ) ) ;
#13504 = DIRECTION ( 'NONE',  ( -1.000000000000000000, -0.000000000000000000, 0.000000000000000000 ) ) ;
#13505 = AXIS2_PLACEMENT_3D ( 'NONE', #16529, #4451, #12711 ) ;
#13506 = CARTESIAN_POINT ( 'NONE',  ( -31.44597781366222122, 56.94165929845684815, 70.50000000000000000 ) ) ;
#13507 = AXIS2_PLACEMENT_3D ( 'NONE', #11757, #3371, #15013 ) ;
#13508 = CARTESIAN_POINT ( 'NONE',  ( 29.37540678000427619, 5.299999999999999822, 7.500000000000000000 ) ) ;
#13509 = ORIENTED_EDGE ( 'NONE', *, *, #12240, .T. ) ;
#13510 = DIRECTION ( 'NONE',  ( -1.000000000000000000, 0.000000000000000000, 0.000000000000000000 ) ) ;
#13511 = CIRCLE ( 'NONE', #7109, 2.299999999999993161 ) ;
#13512 = CARTESIAN_POINT ( 'NONE',  ( 1.724728116533979616, 42.31054587065082728, 43.75876104995653293 ) ) ;
#13513 = DIRECTION ( 'NONE',  ( 0.000000000000000000, 1.000000000000000000, 0.000000000000000000 ) ) ;
#13514 = ORIENTED_EDGE ( 'NONE', *, *, #9427, .T. ) ;
#13515 = DIRECTION ( 'NONE',  ( -1.224646799147353207E-16, -0.000000000000000000, -1.000000000000000000 ) ) ;
#13516 = CIRCLE ( 'NONE', #6755, 0.2500000000000002220 ) ;
#13517 = AXIS2_PLACEMENT_3D ( 'NONE', #18430, #9831, #3114 ) ;
#13518 = ORIENTED_EDGE ( 'NONE', *, *, #9319, .T. ) ;
#13519 = DIRECTION ( 'NONE',  ( 0.000000000000000000, 1.000000000000000000, -0.000000000000000000 ) ) ;
#13520 = EDGE_CURVE ( 'NONE', #818, #2269, #13767, .T. ) ;
#13521 = CARTESIAN_POINT ( 'NONE',  ( 8.641460742840918030, 32.93424481021354921, 68.00000000000000000 ) ) ;
#13522 = ORIENTED_EDGE ( 'NONE', *, *, #3746, .T. ) ;
#13523 = EDGE_CURVE ( 'NONE', #12842, #4642, #3635, .T. ) ;
#13524 = VECTOR ( 'NONE', #18770, 1000.000000000000000 ) ;
#13525 = CIRCLE ( 'NONE', #9193, 0.1000000000000028644 ) ;
#13526 = VERTEX_POINT ( 'NONE', #8322 ) ;
#13527 = TOROIDAL_SURFACE ( 'NONE', #1742, 0.05000000000000000278, 0.05000000000000000278 ) ;
#13528 = CARTESIAN_POINT ( 'NONE',  ( 29.44760881811060926, -2.533476707129126204, 0.1250364218578007836 ) ) ;
#13529 = AXIS2_PLACEMENT_3D ( 'NONE', #17424, #15845, #14062 ) ;
#13530 = ORIENTED_EDGE ( 'NONE', *, *, #2063, .T. ) ;
#13531 = EDGE_CURVE ( 'NONE', #6460, #3943, #19366, .T. ) ;
#13532 = CARTESIAN_POINT ( 'NONE',  ( 1.724728116533979616, 42.31054587065082728, 53.71679706732590631 ) ) ;
#13533 = VERTEX_POINT ( 'NONE', #10338 ) ;
#13534 = DIRECTION ( 'NONE',  ( 1.000000000000000000, 0.000000000000000000, 0.000000000000000000 ) ) ;
#13535 = CIRCLE ( 'NONE', #3906, 2.076718556943725424 ) ;
#13536 = CARTESIAN_POINT ( 'NONE',  ( 15.95292532278785913, -34.11873716947361856, 109.6002446535588319 ) ) ;
#13537 = CARTESIAN_POINT ( 'NONE',  ( -15.95292532278785913, 32.11873716947361856, 68.00000000000000000 ) ) ;
#13538 = DIRECTION ( 'NONE',  ( 0.000000000000000000, -1.000000000000000000, 0.000000000000000000 ) ) ;
#13539 = AXIS2_PLACEMENT_3D ( 'NONE', #10362, #18972, #8682 ) ;
#13540 = CARTESIAN_POINT ( 'NONE',  ( -3.127054932750481964, -33.43424481021354921, 68.00000000000000000 ) ) ;
#13541 = CARTESIAN_POINT ( 'NONE',  ( -32.50000000000002132, -71.00000000000001421, 3.200000000000000178 ) ) ;
#13542 = AXIS2_PLACEMENT_3D ( 'NONE', #8030, #18078, #2434 ) ;
#13543 = CARTESIAN_POINT ( 'NONE',  ( 30.37540678000427619, 6.000000000000000000, 7.200000000000000178 ) ) ;
#13544 = CARTESIAN_POINT ( 'NONE',  ( -1.724728116533986721, 43.31054587065082728, 53.66679706732590915 ) ) ;
#13545 = DIRECTION ( 'NONE',  ( 0.000000000000000000, 0.000000000000000000, 1.000000000000000000 ) ) ;
#13546 = EDGE_CURVE ( 'NONE', #10096, #5643, #12102, .T. ) ;
#13547 = DIRECTION ( 'NONE',  ( 1.000000000000000000, 0.000000000000000000, 0.000000000000000000 ) ) ;
#13548 = ORIENTED_EDGE ( 'NONE', *, *, #3600, .T. ) ;
#13549 = CARTESIAN_POINT ( 'NONE',  ( -1.824728116533986810, 43.26054587065083012, 53.66679706732590915 ) ) ;
#13550 = EDGE_CURVE ( 'NONE', #2930, #21381, #21975, .T. ) ;
#13551 = ORIENTED_EDGE ( 'NONE', *, *, #14276, .F. ) ;
#13552 = ORIENTED_EDGE ( 'NONE', *, *, #1205, .F. ) ;
#13553 = CARTESIAN_POINT ( 'NONE',  ( 31.69597781366222122, 27.99124249474150972, 68.75000000000000000 ) ) ;
#13554 = CARTESIAN_POINT ( 'NONE',  ( 0.000000000000000000, 0.000000000000000000, 82.00000000000000000 ) ) ;
#13555 = ORIENTED_EDGE ( 'NONE', *, *, #1292, .T. ) ;
#13556 = VECTOR ( 'NONE', #17124, 1000.000000000000000 ) ;
#13557 = VERTEX_POINT ( 'NONE', #13450 ) ;
#13558 = PRODUCT_DEFINITION_CONTEXT ( 'detailed design', #14566, 'design' ) ;
#13559 = EDGE_LOOP ( 'NONE', ( #17152, #2465, #12163, #21305 ) ) ;
#13560 = CARTESIAN_POINT ( 'NONE',  ( 0.000000000000000000, -67.54634676501045476, 7.500000000000000000 ) ) ;
#13561 = CARTESIAN_POINT ( 'NONE',  ( -32.20000000000001705, 72.00000000000001421, 3.200000000000000178 ) ) ;
#13562 = ADVANCED_FACE ( 'NONE', ( #6882 ), #5184, .F. ) ;
#13563 = FACE_OUTER_BOUND ( 'NONE', #10147, .T. ) ;
#13564 = ORIENTED_EDGE ( 'NONE', *, *, #3317, .T. ) ;
#13565 = CARTESIAN_POINT ( 'NONE',  ( -30.49999999999999289, -85.00000000000000000, 0.3000000000000002665 ) ) ;
#13566 = AXIS2_PLACEMENT_3D ( 'NONE', #6788, #13586, #48 ) ;
#13567 = MECHANICAL_DESIGN_GEOMETRIC_PRESENTATION_REPRESENTATION (  '', ( #10722 ), #16040 ) ;
#13568 = CARTESIAN_POINT ( 'NONE',  ( -23.02398829872514341, 3.297363125858272070, 13.54387027667929289 ) ) ;
#13569 = AXIS2_PLACEMENT_3D ( 'NONE', #3879, #20990, #602 ) ;
#13570 = CARTESIAN_POINT ( 'NONE',  ( 30.37540678000427619, 0.000000000000000000, 7.200000000000000178 ) ) ;
#13571 = CYLINDRICAL_SURFACE ( 'NONE', #21626, 2.500000000000002220 ) ;
#13572 = ADVANCED_FACE ( 'NONE', ( #3286 ), #20290, .F. ) ;
#13573 = FACE_OUTER_BOUND ( 'NONE', #16100, .T. ) ;
#13574 = ORIENTED_EDGE ( 'NONE', *, *, #6447, .F. ) ;
#13575 = ORIENTED_EDGE ( 'NONE', *, *, #20169, .T. ) ;
#13576 = ORIENTED_EDGE ( 'NONE', *, *, #7913, .T. ) ;
#13577 = DIRECTION ( 'NONE',  ( -0.000000000000000000, -0.000000000000000000, -1.000000000000000000 ) ) ;
#13578 = DIRECTION ( 'NONE',  ( 1.000000000000000000, 0.000000000000000000, 0.000000000000000000 ) ) ;
#13579 = ORIENTED_EDGE ( 'NONE', *, *, #1229, .F. ) ;
#13580 = CARTESIAN_POINT ( 'NONE',  ( -9.178906393579158163, 42.46645089659918426, 67.85468508031152624 ) ) ;
#13581 = CIRCLE ( 'NONE', #3273, 0.5000000000000004441 ) ;
#13582 = CIRCLE ( 'NONE', #12497, 0.4999999999999995559 ) ;
#13583 = CIRCLE ( 'NONE', #15009, 5.299999999999998934 ) ;
#13584 = VERTEX_POINT ( 'NONE', #3506 ) ;
#13585 = CARTESIAN_POINT ( 'NONE',  ( 31.50000000000002132, 71.70000000000001705, 3.200000000000000178 ) ) ;
#13586 = DIRECTION ( 'NONE',  ( 0.000000000000000000, 0.000000000000000000, -1.000000000000000000 ) ) ;
#13587 = ADVANCED_FACE ( 'NONE', ( #3617 ), #17147, .T. ) ;
#13588 = CARTESIAN_POINT ( 'NONE',  ( -1.724728116533986721, 43.26054587065083012, 45.76679706732590347 ) ) ;
#13589 = LINE ( 'NONE', #15379, #8090 ) ;
#13590 = ORIENTED_EDGE ( 'NONE', *, *, #20953, .F. ) ;
#13591 = FACE_OUTER_BOUND ( 'NONE', #2980, .T. ) ;
#13592 = CARTESIAN_POINT ( 'NONE',  ( 14.66174975910705847, -32.10873716947361345, 13.79999999999999893 ) ) ;
#13593 = DIRECTION ( 'NONE',  ( -1.000000000000000000, 0.000000000000000000, 0.000000000000000000 ) ) ;
#13594 = CARTESIAN_POINT ( 'NONE',  ( 1.774728116533979438, 43.31054587065082728, 31.80876104995653719 ) ) ;
#13595 = LINE ( 'NONE', #20436, #3991 ) ;
#13596 = ORIENTED_EDGE ( 'NONE', *, *, #4743, .F. ) ;
#13597 = DIRECTION ( 'NONE',  ( -0.000000000000000000, 1.000000000000000000, -0.000000000000000000 ) ) ;
#13598 = CIRCLE ( 'NONE', #3243, 0.5000000000000004441 ) ;
#13599 = EDGE_CURVE ( 'NONE', #8047, #3329, #16920, .T. ) ;
#13600 = VERTEX_POINT ( 'NONE', #8218 ) ;
#13601 = DIRECTION ( 'NONE',  ( 0.000000000000000000, -0.000000000000000000, -1.000000000000000000 ) ) ;
#13602 = CIRCLE ( 'NONE', #11799, 0.2999999999999947153 ) ;
#13603 = DIRECTION ( 'NONE',  ( 1.000000000000000000, 0.000000000000000000, -0.000000000000000000 ) ) ;
#13604 = EDGE_CURVE ( 'NONE', #12457, #14923, #7216, .T. ) ;
#13605 = DIRECTION ( 'NONE',  ( 0.000000000000000000, 0.000000000000000000, -1.000000000000000000 ) ) ;
#13606 = ORIENTED_EDGE ( 'NONE', *, *, #20598, .T. ) ;
#13607 = ORIENTED_EDGE ( 'NONE', *, *, #2131, .T. ) ;
#13608 = ORIENTED_EDGE ( 'NONE', *, *, #386, .T. ) ;
#13609 = CYLINDRICAL_SURFACE ( 'NONE', #17398, 0.2999999999999999334 ) ;
#13610 = CARTESIAN_POINT ( 'NONE',  ( -14.71174975910705029, 52.11873716947361856, 14.00000000000000000 ) ) ;
#13611 = ORIENTED_EDGE ( 'NONE', *, *, #14962, .F. ) ;
#13612 = ORIENTED_EDGE ( 'NONE', *, *, #4459, .F. ) ;
#13613 = LINE ( 'NONE', #4894, #11468 ) ;
#13614 = EDGE_CURVE ( 'NONE', #15826, #119, #8759, .T. ) ;
#13615 = VERTEX_POINT ( 'NONE', #17476 ) ;
#13616 = CARTESIAN_POINT ( 'NONE',  ( -1.724728116533986721, 43.31054587065082728, 31.75876104995653648 ) ) ;
#13617 = AXIS2_PLACEMENT_3D ( 'NONE', #16894, #21944, #13420 ) ;
#13618 = CARTESIAN_POINT ( 'NONE',  ( -9.641460742840918030, 32.61873716947361856, 68.00000000000000000 ) ) ;
#13619 = CARTESIAN_POINT ( 'NONE',  ( 4.127054932750481520, 32.93424481021354921, 42.50000000000000000 ) ) ;
#13620 = LINE ( 'NONE', #18547, #193 ) ;
#13621 = ORIENTED_EDGE ( 'NONE', *, *, #13050, .T. ) ;
#13622 = CYLINDRICAL_SURFACE ( 'NONE', #11630, 0.2999999999999999334 ) ;
#13623 = FACE_OUTER_BOUND ( 'NONE', #12661, .T. ) ;
#13624 = CARTESIAN_POINT ( 'NONE',  ( 26.56227312273159313, 9.958410664601840878, 13.79999999999999893 ) ) ;
#13625 = ORIENTED_EDGE ( 'NONE', *, *, #1267, .F. ) ;
#13626 = LINE ( 'NONE', #16634, #18043 ) ;
#13627 = ADVANCED_FACE ( 'NONE', ( #7304 ), #21187, .F. ) ;
#13628 = MECHANICAL_DESIGN_GEOMETRIC_PRESENTATION_REPRESENTATION (  '', ( #19036 ), #12885 ) ;
#13629 = CIRCLE ( 'NONE', #13964, 0.04999999999999991257 ) ;
#13630 = EDGE_CURVE ( 'NONE', #19361, #11011, #15885, .T. ) ;
#13631 = ORIENTED_EDGE ( 'NONE', *, *, #11151, .T. ) ;
#13633 = ADVANCED_FACE ( 'NONE', ( #14222 ), #15557, .T. ) ;
#13632 = DIRECTION ( 'NONE',  ( -1.000000000000000000, 0.000000000000000000, -0.000000000000000000 ) ) ;
#13634 = FACE_OUTER_BOUND ( 'NONE', #15225, .T. ) ;
#13635 = ORIENTED_EDGE ( 'NONE', *, *, #13667, .T. ) ;
#13636 = LINE ( 'NONE', #22046, #17760 ) ;
#13637 = ORIENTED_EDGE ( 'NONE', *, *, #16057, .F. ) ;
#13638 = AXIS2_PLACEMENT_3D ( 'NONE', #16696, #12994, #11105 ) ;
#13639 = DIRECTION ( 'NONE',  ( -0.000000000000000000, -1.000000000000000000, -0.000000000000000000 ) ) ;
#13640 = ORIENTED_EDGE ( 'NONE', *, *, #13784, .F. ) ;
#13641 = AXIS2_PLACEMENT_3D ( 'NONE', #10114, #18717, #16923 ) ;
#13642 = CYLINDRICAL_SURFACE ( 'NONE', #1874, 4.351418481279133665 ) ;
#13643 = DIRECTION ( 'NONE',  ( 0.000000000000000000, 1.000000000000000000, 0.000000000000000000 ) ) ;
#13644 = EDGE_CURVE ( 'NONE', #1252, #15889, #13652, .T. ) ;
#13645 = DIRECTION ( 'NONE',  ( 0.000000000000000000, -1.000000000000000000, 0.000000000000000000 ) ) ;
#13646 = CARTESIAN_POINT ( 'NONE',  ( -1.724728116533986721, 42.31054587065082728, 51.75876104995654003 ) ) ;
#13647 = CARTESIAN_POINT ( 'NONE',  ( -24.00488095381848197, 42.46645089659918426, 13.49999999999999822 ) ) ;
#13648 = DIRECTION ( 'NONE',  ( 0.000000000000000000, 0.000000000000000000, -1.000000000000000000 ) ) ;
#13649 = CARTESIAN_POINT ( 'NONE',  ( -3.627054932750481964, -32.93424481021354921, 42.50000000000000000 ) ) ;
#13650 = ADVANCED_FACE ( 'NONE', ( #13999 ), #14097, .T. ) ;
#13651 = ORIENTED_EDGE ( 'NONE', *, *, #1419, .F. ) ;
#13652 = CIRCLE ( 'NONE', #4721, 0.1000000000000028644 ) ;
#13653 = DIRECTION ( 'NONE',  ( -1.000000000000000000, -3.543406725251269872E-15, 1.224646799147353207E-16 ) ) ;
#13654 = CARTESIAN_POINT ( 'NONE',  ( 0.000000000000000000, -38.74634676501045760, 42.50000000000000000 ) ) ;
#13655 = AXIS2_PLACEMENT_3D ( 'NONE', #14965, #6491, #13284 ) ;
#13656 = FACE_OUTER_BOUND ( 'NONE', #21758, .T. ) ;
#13657 = VERTEX_POINT ( 'NONE', #19053 ) ;
#13658 = ORIENTED_EDGE ( 'NONE', *, *, #4174, .F. ) ;
#13659 = DIRECTION ( 'NONE',  ( 0.000000000000000000, 0.000000000000000000, 1.000000000000000000 ) ) ;
#13660 = ORIENTED_EDGE ( 'NONE', *, *, #19001, .F. ) ;
#13661 =( NAMED_UNIT ( * ) SI_UNIT ( $, .STERADIAN. ) SOLID_ANGLE_UNIT ( ) );
#13662 = ORIENTED_EDGE ( 'NONE', *, *, #18692, .T. ) ;
#13663 = ORIENTED_EDGE ( 'NONE', *, *, #6432, .T. ) ;
#13664 = EDGE_CURVE ( 'NONE', #21087, #17432, #2028, .T. ) ;
#13665 = CYLINDRICAL_SURFACE ( 'NONE', #2346, 0.2500000000000002220 ) ;
#13666 = CYLINDRICAL_SURFACE ( 'NONE', #967, 0.05000000000000143219 ) ;
#13667 = EDGE_CURVE ( 'NONE', #2670, #18749, #21169, .T. ) ;
#13668 = CARTESIAN_POINT ( 'NONE',  ( 13.37248138918699425, 42.46645089659917716, 69.50000000000000000 ) ) ;
#13669 = CARTESIAN_POINT ( 'NONE',  ( 0.000000000000000000, 52.11873716947361856, 109.6002446535588319 ) ) ;
#13670 = CARTESIAN_POINT ( 'NONE',  ( -23.02398829872513986, 3.004888651530577715, 13.74579066068641708 ) ) ;
#13671 = CARTESIAN_POINT ( 'NONE',  ( 0.000000000000000000, -52.39333383871510108, 13.79999999999999893 ) ) ;
#13672 = DIRECTION ( 'NONE',  ( -0.000000000000000000, 0.000000000000000000, 1.000000000000000000 ) ) ;
#13673 = CARTESIAN_POINT ( 'NONE',  ( -29.13662752439705272, 0.000000000000000000, 13.50000000000000000 ) ) ;
#13674 = ORIENTED_EDGE ( 'NONE', *, *, #13198, .T. ) ;
#13675 = EDGE_LOOP ( 'NONE', ( #18777, #3583, #11914, #16485 ) ) ;
#13676 = ORIENTED_EDGE ( 'NONE', *, *, #8718, .T. ) ;
#13677 = CARTESIAN_POINT ( 'NONE',  ( 14.96174975910705918, 41.81054587065082728, 13.80000000000001315 ) ) ;
#13678 = FILL_AREA_STYLE_COLOUR ( '', #12610 ) ;
#13679 = DIRECTION ( 'NONE',  ( 0.000000000000000000, 0.000000000000000000, 1.000000000000000000 ) ) ;
#13680 = VERTEX_POINT ( 'NONE', #7095 ) ;
#13681 = EDGE_CURVE ( 'NONE', #15917, #19413, #9742, .T. ) ;
#13682 = CARTESIAN_POINT ( 'NONE',  ( -23.36078716634399655, 44.83461903493144973, 68.25000000000000000 ) ) ;
#13683 = DIRECTION ( 'NONE',  ( 1.000000000000000000, 0.000000000000000000, 0.000000000000000000 ) ) ;
#13684 = DIRECTION ( 'NONE',  ( 0.000000000000000000, 0.000000000000000000, 1.000000000000000000 ) ) ;
#13685 = CARTESIAN_POINT ( 'NONE',  ( -11.62890639357915923, 43.00645089659917630, 70.88527860057354246 ) ) ;
#13686 = CARTESIAN_POINT ( 'NONE',  ( 1.724728116533979838, 43.31054587065082728, 41.71679706732590631 ) ) ;
#13687 = EDGE_LOOP ( 'NONE', ( #6639, #3397, #3751, #6672 ) ) ;
#13688 = CARTESIAN_POINT ( 'NONE',  ( 1.824728116533979261, 43.31054587065082728, 27.80876104995653719 ) ) ;
#13689 = FACE_OUTER_BOUND ( 'NONE', #19211, .T. ) ;
#13690 = CYLINDRICAL_SURFACE ( 'NONE', #16128, 0.2999999999999999334 ) ;
#13691 = DIRECTION ( 'NONE',  ( 0.000000000000000000, 0.000000000000000000, 1.000000000000000000 ) ) ;
#13692 = EDGE_LOOP ( 'NONE', ( #2712, #19362, #19458, #19314 ) ) ;
#13693 = LINE ( 'NONE', #17172, #19868 ) ;
#13694 = CARTESIAN_POINT ( 'NONE',  ( -1.724728116533986721, 42.36054587065083155, 37.71679706732590631 ) ) ;
#13695 = ORIENTED_EDGE ( 'NONE', *, *, #11664, .F. ) ;
#13696 = DIRECTION ( 'NONE',  ( -1.000000000000000000, 0.000000000000000000, 0.000000000000000000 ) ) ;
#13697 = DIRECTION ( 'NONE',  ( 1.000000000000000000, -0.000000000000000000, 0.000000000000000000 ) ) ;
#13698 = DIRECTION ( 'NONE',  ( 1.301042606982568087E-14, 0.000000000000000000, 1.000000000000000000 ) ) ;
#13699 = ORIENTED_EDGE ( 'NONE', *, *, #5765, .F. ) ;
#13700 = ORIENTED_EDGE ( 'NONE', *, *, #15498, .T. ) ;
#13701 = EDGE_LOOP ( 'NONE', ( #4593, #15978, #21538, #17283 ) ) ;
#13702 = DIRECTION ( 'NONE',  ( 0.000000000000000000, 0.000000000000000000, 1.000000000000000000 ) ) ;
#13703 = EDGE_CURVE ( 'NONE', #15847, #13894, #16508, .T. ) ;
#13704 = DIRECTION ( 'NONE',  ( 1.000000000000000000, 0.000000000000000000, 0.000000000000000000 ) ) ;
#13705 = DIRECTION ( 'NONE',  ( 0.000000000000000000, 1.000000000000000000, 0.000000000000000000 ) ) ;
#13706 = ORIENTED_EDGE ( 'NONE', *, *, #13387, .T. ) ;
#13707 = CARTESIAN_POINT ( 'NONE',  ( 1.724728116533979616, 43.31054587065082728, 47.75876104995653293 ) ) ;
#13708 = EDGE_CURVE ( 'NONE', #9069, #5223, #352, .T. ) ;
#13709 = ORIENTED_EDGE ( 'NONE', *, *, #19801, .T. ) ;
#13710 = FACE_OUTER_BOUND ( 'NONE', #13901, .T. ) ;
#13711 = ADVANCED_FACE ( 'NONE', ( #14331 ), #3953, .T. ) ;
#13712 = CARTESIAN_POINT ( 'NONE',  ( -1.774728116533986544, 42.31054587065082728, 43.80876104995653719 ) ) ;
#13713 = DIRECTION ( 'NONE',  ( -1.000000000000000000, 0.000000000000000000, 0.000000000000000000 ) ) ;
#13714 = DIRECTION ( 'NONE',  ( -0.000000000000000000, 0.000000000000000000, 1.000000000000000000 ) ) ;
#13715 = ORIENTED_EDGE ( 'NONE', *, *, #6818, .T. ) ;
#13716 = CARTESIAN_POINT ( 'NONE',  ( 23.02398829872513986, 3.297879325581059451, 13.54382403646204480 ) ) ;
#13717 =( REPRESENTATION_RELATIONSHIP ('NONE','NONE', #561, #9142 ) REPRESENTATION_RELATIONSHIP_WITH_TRANSFORMATION ( #15870 )SHAPE_REPRESENTATION_RELATIONSHIP( ) );
#13718 = DIRECTION ( 'NONE',  ( -1.000000000000000000, 0.000000000000000000, -0.000000000000000000 ) ) ;
#13719 = DIRECTION ( 'NONE',  ( 1.000000000000000000, 0.000000000000000000, 0.000000000000000000 ) ) ;
#13720 = ORIENTED_EDGE ( 'NONE', *, *, #6644, .T. ) ;
#13721 = ORIENTED_EDGE ( 'NONE', *, *, #8726, .F. ) ;
#13722 = FACE_OUTER_BOUND ( 'NONE', #17082, .T. ) ;
#13723 = LINE ( 'NONE', #16979, #5250 ) ;
#13724 = ORIENTED_EDGE ( 'NONE', *, *, #20680, .F. ) ;
#13725 = DIRECTION ( 'NONE',  ( 0.000000000000000000, 0.000000000000000000, 1.000000000000000000 ) ) ;
#13726 = EDGE_CURVE ( 'NONE', #11031, #5468, #17217, .T. ) ;
#13727 = ORIENTED_EDGE ( 'NONE', *, *, #13017, .T. ) ;
#13728 = DIRECTION ( 'NONE',  ( 0.000000000000000000, 0.000000000000000000, 1.000000000000000000 ) ) ;
#13729 = ORIENTED_EDGE ( 'NONE', *, *, #9215, .F. ) ;
#13730 = VECTOR ( 'NONE', #5078, 1000.000000000000000 ) ;
#13731 = EDGE_CURVE ( 'NONE', #11808, #10741, #6898, .T. ) ;
#13732 = FACE_OUTER_BOUND ( 'NONE', #6606, .T. ) ;
#13733 = VERTEX_POINT ( 'NONE', #455 ) ;
#13734 = CARTESIAN_POINT ( 'NONE',  ( -29.48732477999263679, 2.488184282963944671, 0.2032176586593637813 ) ) ;
#13735 = ADVANCED_FACE ( 'NONE', ( #10658 ), #3720, .T. ) ;
#13736 = DIRECTION ( 'NONE',  ( 1.000000000000000000, 0.000000000000000000, 0.000000000000000000 ) ) ;
#13737 = ADVANCED_FACE ( 'NONE', ( #19383 ), #4052, .T. ) ;
#13738 = DIRECTION ( 'NONE',  ( 1.000000000000000000, 0.000000000000000000, 0.000000000000000000 ) ) ;
#13739 = LINE ( 'NONE', #11618, #10356 ) ;
#13740 = CARTESIAN_POINT ( 'NONE',  ( -14.66174975910705136, -51.76873716947361714, 13.50000000000000000 ) ) ;
#13741 = AXIS2_PLACEMENT_3D ( 'NONE', #16510, #21350, #18306 ) ;
#13742 = CIRCLE ( 'NONE', #18766, 0.2999999999999999334 ) ;
#13743 = ORIENTED_EDGE ( 'NONE', *, *, #18942, .F. ) ;
#13744 = EDGE_CURVE ( 'NONE', #440, #5258, #14876, .T. ) ;
#13745 = DIRECTION ( 'NONE',  ( 0.000000000000000000, 0.000000000000000000, -1.000000000000000000 ) ) ;
#13746 = CARTESIAN_POINT ( 'NONE',  ( -11.94625475753432120, -2.835528047479821900, 68.50000000000000000 ) ) ;
#13747 = PRODUCT_DEFINITION_SHAPE ( 'NONE', 'NONE',  #22174 ) ;
#13748 = VERTEX_POINT ( 'NONE', #1121 ) ;
#13749 = VERTEX_POINT ( 'NONE', #7864 ) ;
#13750 = LINE ( 'NONE', #9868, #14235 ) ;
#13751 = DIRECTION ( 'NONE',  ( 1.000000000000000000, 0.000000000000000000, 0.000000000000000000 ) ) ;
#13752 = EDGE_CURVE ( 'NONE', #4126, #3783, #3296, .T. ) ;
#13753 = ORIENTED_EDGE ( 'NONE', *, *, #17002, .F. ) ;
#13754 =( LENGTH_UNIT ( ) NAMED_UNIT ( * ) SI_UNIT ( .MILLI., .METRE. ) );
#13755 = AXIS2_PLACEMENT_3D ( 'NONE', #20235, #5136, #4798 ) ;
#13756 = VERTEX_POINT ( 'NONE', #18015 ) ;
#13757 = AXIS2_PLACEMENT_3D ( 'NONE', #7125, #20660, #1943 ) ;
#13758 = VECTOR ( 'NONE', #19300, 1000.000000000000000 ) ;
#13759 = AXIS2_PLACEMENT_3D ( 'NONE', #14474, #21335, #9579 ) ;
#13760 = ORIENTED_EDGE ( 'NONE', *, *, #12823, .T. ) ;
#13761 = EDGE_CURVE ( 'NONE', #17, #18889, #6076, .T. ) ;
#13762 = DIRECTION ( 'NONE',  ( -0.000000000000000000, -0.000000000000000000, 1.000000000000000000 ) ) ;
#13763 = CARTESIAN_POINT ( 'NONE',  ( -9.141460742840918030, 33.43424481021354921, 7.321391277662001151 ) ) ;
#13764 = FACE_OUTER_BOUND ( 'NONE', #1721, .T. ) ;
#13765 =( LENGTH_UNIT ( ) NAMED_UNIT ( * ) SI_UNIT ( .MILLI., .METRE. ) );
#13766 = DIRECTION ( 'NONE',  ( -0.000000000000000000, 1.000000000000000000, 0.000000000000000000 ) ) ;
#13767 = LINE ( 'NONE', #18605, #16492 ) ;
#13768 = CARTESIAN_POINT ( 'NONE',  ( -1.774728116533986766, 42.36054587065083155, 27.80876104995653719 ) ) ;
#13769 = DIRECTION ( 'NONE',  ( -0.000000000000000000, 1.000000000000000000, -0.000000000000000000 ) ) ;
#13770 = CIRCLE ( 'NONE', #10929, 0.2999999999999999334 ) ;
#13771 = VECTOR ( 'NONE', #21967, 1000.000000000000000 ) ;
#13772 = CARTESIAN_POINT ( 'NONE',  ( -30.67540678000428045, -63.74634676501045050, 3.500000000000000000 ) ) ;
#13773 = VECTOR ( 'NONE', #17345, 1000.000000000000000 ) ;
#13774 = ORIENTED_EDGE ( 'NONE', *, *, #8552, .T. ) ;
#13775 = CIRCLE ( 'NONE', #19895, 0.2999999999999999334 ) ;
#13776 = EDGE_LOOP ( 'NONE', ( #16459, #20014, #16938, #21547 ) ) ;
#13777 = DIRECTION ( 'NONE',  ( -1.000000000000000000, 0.000000000000000000, 0.000000000000000000 ) ) ;
#13779 = ADVANCED_FACE ( 'NONE', ( #16333 ), #21623, .T. ) ;
#13778 = CARTESIAN_POINT ( 'NONE',  ( -33.50000000000001421, 84.70000000000001705, 78.20000000000000284 ) ) ;
#13780 = ORIENTED_EDGE ( 'NONE', *, *, #11893, .T. ) ;
#13781 = EDGE_CURVE ( 'NONE', #1826, #14518, #89, .T. ) ;
#13782 = ORIENTED_EDGE ( 'NONE', *, *, #8425, .F. ) ;
#13784 = EDGE_CURVE ( 'NONE', #8405, #8427, #6189, .T. ) ;
#13783 = CARTESIAN_POINT ( 'NONE',  ( -33.20000000000001705, 85.00000000000000000, 78.50000000000000000 ) ) ;
#13785 = AXIS2_PLACEMENT_3D ( 'NONE', #7965, #12966, #17901 ) ;
#13786 = CIRCLE ( 'NONE', #2732, 0.2999999999999999889 ) ;
#13787 = CIRCLE ( 'NONE', #6313, 0.2999999999999999334 ) ;
#13788 = DIRECTION ( 'NONE',  ( -1.000000000000000000, 0.000000000000000000, 0.000000000000000000 ) ) ;
#13789 = DIRECTION ( 'NONE',  ( 0.9729678061520314891, 0.2309407893632107189, 0.000000000000000000 ) ) ;
#13790 = CIRCLE ( 'NONE', #13094, 0.5000000000000004441 ) ;
#13791 = ORIENTED_EDGE ( 'NONE', *, *, #16895, .F. ) ;
#13792 = DIRECTION ( 'NONE',  ( 1.000000000000000000, 0.000000000000000000, 0.000000000000000000 ) ) ;
#13793 = DIRECTION ( 'NONE',  ( 2.388292521039847891E-16, 0.000000000000000000, 1.000000000000000000 ) ) ;
#13794 = DIRECTION ( 'NONE',  ( 0.000000000000000000, 1.000000000000000000, 0.000000000000000000 ) ) ;
#13795 = FACE_OUTER_BOUND ( 'NONE', #12618, .T. ) ;
#13796 = CARTESIAN_POINT ( 'NONE',  ( 26.37540678000427619, 10.94079601157914539, 13.50000000000000000 ) ) ;
#13797 = PRODUCT_RELATED_PRODUCT_CATEGORY ( 'part', '', ( #11428 ) ) ;
#13798 = CARTESIAN_POINT ( 'NONE',  ( 15.95292532278785913, -32.61873716947361856, 68.00000000000000000 ) ) ;
#13799 = DIRECTION ( 'NONE',  ( 0.000000000000000000, 0.000000000000000000, 1.000000000000000000 ) ) ;
#13800 = PLANE ( 'NONE',  #2685 ) ;
#13801 = CARTESIAN_POINT ( 'NONE',  ( 1.724728116533979838, 43.26054587065083012, 37.71679706732590631 ) ) ;
#13802 = CIRCLE ( 'NONE', #9897, 0.2500000000000002220 ) ;
#13803 = EDGE_LOOP ( 'NONE', ( #9164, #9784, #5481, #10673 ) ) ;
#13804 = AXIS2_PLACEMENT_3D ( 'NONE', #13475, #15148, #17168 ) ;
#13805 = AXIS2_PLACEMENT_3D ( 'NONE', #11693, #7126, #10370 ) ;
#13806 = EDGE_LOOP ( 'NONE', ( #7867, #4781, #4281, #4699 ) ) ;
#13807 = ORIENTED_EDGE ( 'NONE', *, *, #4083, .T. ) ;
#13808 = DIRECTION ( 'NONE',  ( -6.123233995736766036E-17, 0.000000000000000000, 1.000000000000000000 ) ) ;
#13809 = DIRECTION ( 'NONE',  ( 1.000000000000000000, -3.052134192567367925E-16, 0.000000000000000000 ) ) ;
#13810 = EDGE_CURVE ( 'NONE', #21351, #10680, #21736, .T. ) ;
#13811 = CARTESIAN_POINT ( 'NONE',  ( -15.95292532278785913, 32.61873716947361856, 68.50000000000000000 ) ) ;
#13812 = VECTOR ( 'NONE', #8162, 1000.000000000000000 ) ;
#13813 = ADVANCED_FACE ( 'NONE', ( #1014 ), #9415, .T. ) ;
#13814 = DIRECTION ( 'NONE',  ( 0.000000000000000000, 0.000000000000000000, 1.000000000000000000 ) ) ;
#13815 = CIRCLE ( 'NONE', #7764, 4.193574995607837863 ) ;
#13816 = ORIENTED_EDGE ( 'NONE', *, *, #21805, .F. ) ;
#13817 = CARTESIAN_POINT ( 'NONE',  ( -21.92816239687475743, 42.46645089659918426, 13.50000000000000000 ) ) ;
#13818 = VERTEX_POINT ( 'NONE', #13209 ) ;
#13819 = DIRECTION ( 'NONE',  ( 1.000000000000000000, 0.000000000000000000, 0.000000000000000000 ) ) ;
#13820 = DIRECTION ( 'NONE',  ( 0.000000000000000000, 0.000000000000000000, 1.000000000000000000 ) ) ;
#13821 = CLOSED_SHELL ( 'NONE', ( #15509, #6668, #2174, #13038, #16519, #14067, #3963, #3062, #12263, #13068, #10361, #17164, #603, #13438, #5805, #20658, #7804, #12369, #5865, #5470, #6093, #20836, #20982, #902, #8654, #8419, #20631, #11705, #656, #1646, #3196, #3646, #12122, #14419 ) ) ;
#13822 = AXIS2_PLACEMENT_3D ( 'NONE', #13193, #18786, #14984 ) ;
#13823 = AXIS2_PLACEMENT_3D ( 'NONE', #15490, #7012, #20662 ) ;
#13824 = DIRECTION ( 'NONE',  ( -1.000000000000000000, 0.000000000000000000, 0.000000000000000000 ) ) ;
#13825 = DIRECTION ( 'NONE',  ( 0.000000000000000000, 1.000000000000000000, 0.000000000000000000 ) ) ;
#13826 = ORIENTED_EDGE ( 'NONE', *, *, #20870, .F. ) ;
#13827 = CARTESIAN_POINT ( 'NONE',  ( 23.02398829872514341, 2.388551872609025573, 13.39771463486666470 ) ) ;
#13828 = CARTESIAN_POINT ( 'NONE',  ( 17.95292532278785913, 50.11873716947361856, 68.00000000000000000 ) ) ;
#13829 = CIRCLE ( 'NONE', #12059, 0.6000000000000033085 ) ;
#13830 = SPHERICAL_SURFACE ( 'NONE', #1202, 0.5000000000000000000 ) ;
#13831 = CARTESIAN_POINT ( 'NONE',  ( -21.92816239687475743, 42.46645089659918426, 13.74999999999999822 ) ) ;
#13832 = ORIENTED_EDGE ( 'NONE', *, *, #20121, .T. ) ;
#13833 = ADVANCED_FACE ( 'NONE', ( #4717 ), #12567, .F. ) ;
#13834 = FACE_OUTER_BOUND ( 'NONE', #15566, .T. ) ;
#13835 = AXIS2_PLACEMENT_3D ( 'NONE', #19980, #2959, #19853 ) ;
#13836 = DIRECTION ( 'NONE',  ( 2.832483164223434527E-16, -1.000000000000000000, 0.000000000000000000 ) ) ;
#13837 =( BOUNDED_CURVE ( )  B_SPLINE_CURVE ( 3, ( #11164, #7610, #2780, #4454 ),
 .UNSPECIFIED., .F., .T. ) 
 B_SPLINE_CURVE_WITH_KNOTS ( ( 4, 4 ),
 ( 1.570796326794896558, 3.141592653589793116 ),
 .UNSPECIFIED. ) 
 CURVE ( )  GEOMETRIC_REPRESENTATION_ITEM ( )  RATIONAL_B_SPLINE_CURVE ( ( 1.000000000000000000, 0.8047378541243649375, 0.8047378541243649375, 1.000000000000000000 ) ) 
 REPRESENTATION_ITEM ( '' )  );
#13838 = ORIENTED_EDGE ( 'NONE', *, *, #11310, .T. ) ;
#13839 = ADVANCED_FACE ( 'NONE', ( #14660 ), #12971, .T. ) ;
#13840 = DIRECTION ( 'NONE',  ( -1.000000000000000000, 0.000000000000000000, 0.000000000000000000 ) ) ;
#13841 = EDGE_LOOP ( 'NONE', ( #12688, #5625, #436, #6968 ) ) ;
#13842 = VECTOR ( 'NONE', #11612, 1000.000000000000000 ) ;
#13843 = AXIS2_PLACEMENT_3D ( 'NONE', #17118, #15640, #18913 ) ;
#13844 = AXIS2_PLACEMENT_3D ( 'NONE', #10748, #10633, #19256 ) ;
#13845 = ORIENTED_EDGE ( 'NONE', *, *, #4772, .F. ) ;
#13846 = AXIS2_PLACEMENT_3D ( 'NONE', #7241, #3659, #19199 ) ;
#13847 = ORIENTED_EDGE ( 'NONE', *, *, #11838, .F. ) ;
#13848 = AXIS2_PLACEMENT_3D ( 'NONE', #12210, #5759, #5860 ) ;
#13849 = APPLICATION_CONTEXT ( 'automotive_design' ) ;
#13850 = ORIENTED_EDGE ( 'NONE', *, *, #12918, .F. ) ;
#13851 = DIRECTION ( 'NONE',  ( 0.000000000000000000, 0.000000000000000000, 1.000000000000000000 ) ) ;
#13852 = DIRECTION ( 'NONE',  ( 1.000000000000000000, -0.000000000000000000, 6.123233995736764803E-17 ) ) ;
#13853 = DIRECTION ( 'NONE',  ( 0.000000000000000000, 0.000000000000000000, 1.000000000000000000 ) ) ;
#13854 = EDGE_CURVE ( 'NONE', #9360, #398, #15444, .T. ) ;
#13855 = DIRECTION ( 'NONE',  ( -1.000000000000000000, 0.000000000000000000, 0.000000000000000000 ) ) ;
#13856 = UNCERTAINTY_MEASURE_WITH_UNIT (LENGTH_MEASURE( 1.000000000000000082E-05 ), #7209, 'distance_accuracy_value', 'NONE');
#13857 = AXIS2_PLACEMENT_3D ( 'NONE', #8363, #15295, #20346 ) ;
#13858 = VECTOR ( 'NONE', #11603, 1000.000000000000000 ) ;
#13859 = CARTESIAN_POINT ( 'NONE',  ( 29.50000000000002132, 2.512390033608338236, 0.2999999999999947153 ) ) ;
#13860 = CARTESIAN_POINT ( 'NONE',  ( 0.000000000000000000, 0.000000000000000000, 1.500000000000000000 ) ) ;
#13861 = TOROIDAL_SURFACE ( 'NONE', #15297, 2.800000000000002043, 0.2999999999999999889 ) ;
#13862 = DIRECTION ( 'NONE',  ( -1.000000000000000000, 0.000000000000000000, 0.000000000000000000 ) ) ;
#13863 = VECTOR ( 'NONE', #21058, 1000.000000000000000 ) ;
#13864 = AXIS2_PLACEMENT_3D ( 'NONE', #15829, #21121, #2522 ) ;
#13865 = ORIENTED_EDGE ( 'NONE', *, *, #19492, .F. ) ;
#13866 = ADVANCED_FACE ( 'NONE', ( #14544 ), #19820, .T. ) ;
#13867 = DIRECTION ( 'NONE',  ( 0.000000000000000000, 0.000000000000000000, -1.000000000000000000 ) ) ;
#13868 = CARTESIAN_POINT ( 'NONE',  ( 0.000000000000000000, -71.70000000000001705, 1.800000000000000044 ) ) ;
#13869 = EDGE_CURVE ( 'NONE', #2970, #9771, #20811, .T. ) ;
#13870 = ORIENTED_EDGE ( 'NONE', *, *, #9955, .F. ) ;
#13871 = ORIENTED_EDGE ( 'NONE', *, *, #13869, .F. ) ;
#13872 = PLANE ( 'NONE',  #2813 ) ;
#13873 = EDGE_CURVE ( 'NONE', #16490, #2211, #5958, .T. ) ;
#13874 = APPLICATION_PROTOCOL_DEFINITION ( 'draft international standard', 'automotive_design', 1998, #12566 ) ;
#13875 = EDGE_LOOP ( 'NONE', ( #17854, #15314, #8099 ) ) ;
#13876 = AXIS2_PLACEMENT_3D ( 'NONE', #8163, #21818, #9731 ) ;
#13877 = CARTESIAN_POINT ( 'NONE',  ( 23.02398829872514341, -2.334689865870722691, 13.36916081092389241 ) ) ;
#13878 = VERTEX_POINT ( 'NONE', #2816 ) ;
#13879 = AXIS2_PLACEMENT_3D ( 'NONE', #13179, #21814, #9828 ) ;
#13880 = ORIENTED_EDGE ( 'NONE', *, *, #10868, .F. ) ;
#13881 = CIRCLE ( 'NONE', #22129, 0.6999999999999992895 ) ;
#13882 = DIRECTION ( 'NONE',  ( 0.000000000000000000, -1.000000000000000000, 0.000000000000000000 ) ) ;
#13883 = PLANE ( 'NONE',  #18075 ) ;
#13884 = ADVANCED_FACE ( 'NONE', ( #7970 ), #16454, .F. ) ;
#13885 = FACE_OUTER_BOUND ( 'NONE', #275, .T. ) ;
#13886 = CARTESIAN_POINT ( 'NONE',  ( 23.02398829872513986, 3.528912754968628551, 13.79999999999999893 ) ) ;
#13887 = DIRECTION ( 'NONE',  ( 0.000000000000000000, 0.000000000000000000, -1.000000000000000000 ) ) ;
#13888 = CARTESIAN_POINT ( 'NONE',  ( -29.37540678000427619, -5.299999999999999822, 7.200000000000000178 ) ) ;
#13889 = DIRECTION ( 'NONE',  ( 6.123233995736764803E-17, 0.000000000000000000, -1.000000000000000000 ) ) ;
#13890 = CARTESIAN_POINT ( 'NONE',  ( -9.641460742840918030, -32.11873716947361856, 68.00000000000000000 ) ) ;
#13891 = CARTESIAN_POINT ( 'NONE',  ( -14.96174975910705207, -51.86873716947361856, 68.00000000000000000 ) ) ;
#13892 = VECTOR ( 'NONE', #9103, 1000.000000000000000 ) ;
#13893 = EDGE_CURVE ( 'NONE', #11579, #5463, #3655, .T. ) ;
#13894 = VERTEX_POINT ( 'NONE', #11960 ) ;
#13895 = ORIENTED_EDGE ( 'NONE', *, *, #15603, .T. ) ;
#13896 = DIRECTION ( 'NONE',  ( 0.000000000000000000, 0.000000000000000000, 1.000000000000000000 ) ) ;
#13897 = ADVANCED_FACE ( 'NONE', ( #113 ), #20152, .F. ) ;
#13898 = AXIS2_PLACEMENT_3D ( 'NONE', #9282, #10032, #4359 ) ;
#13899 = FILL_AREA_STYLE ('',( #13678 ) ) ;
#13900 = DIRECTION ( 'NONE',  ( -0.000000000000000000, -1.000000000000000000, -0.000000000000000000 ) ) ;
#13901 = EDGE_LOOP ( 'NONE', ( #2371, #7182, #21594, #13922 ) ) ;
#13902 = PLANE ( 'NONE',  #20951 ) ;
#13903 = DIRECTION ( 'NONE',  ( 0.000000000000000000, 0.000000000000000000, 1.000000000000000000 ) ) ;
#13904 = AXIS2_PLACEMENT_3D ( 'NONE', #12828, #7702, #14505 ) ;
#13905 = CARTESIAN_POINT ( 'NONE',  ( -31.50000000000002132, 72.00000000000001421, 3.200000000000000178 ) ) ;
#13906 = CIRCLE ( 'NONE', #17144, 2.000000000000001776 ) ;
#13907 = AXIS2_PLACEMENT_3D ( 'NONE', #15066, #5228, #6585 ) ;
#13908 = CARTESIAN_POINT ( 'NONE',  ( 8.641460742840918030, -32.93424481021354921, 68.00000000000000000 ) ) ;
#13909 = VERTEX_POINT ( 'NONE', #6961 ) ;
#13910 = DIRECTION ( 'NONE',  ( 0.000000000000000000, 0.000000000000000000, 1.000000000000000000 ) ) ;
#13911 = CARTESIAN_POINT ( 'NONE',  ( 30.67540678000428045, -6.000000000000000000, 3.799999999999999822 ) ) ;
#13912 = EDGE_CURVE ( 'NONE', #9447, #2103, #16124, .T. ) ;
#13913 = DIRECTION ( 'NONE',  ( 0.000000000000000000, 0.000000000000000000, -1.000000000000000000 ) ) ;
#13914 = CARTESIAN_POINT ( 'NONE',  ( 14.96174975910707161, 51.61873716947361856, 68.25000000000000000 ) ) ;
#13915 =( NAMED_UNIT ( * ) SI_UNIT ( $, .STERADIAN. ) SOLID_ANGLE_UNIT ( ) );
#13916 = FACE_OUTER_BOUND ( 'NONE', #1410, .T. ) ;
#13917 = EDGE_LOOP ( 'NONE', ( #15696, #3609, #21800, #4831 ) ) ;
#13918 = FACE_OUTER_BOUND ( 'NONE', #142, .T. ) ;
#13919 = DIRECTION ( 'NONE',  ( -0.000000000000000000, -0.000000000000000000, -1.000000000000000000 ) ) ;
#13920 = DIRECTION ( 'NONE',  ( 1.000000000000000000, 0.000000000000000000, 0.000000000000000000 ) ) ;
#13921 = VERTEX_POINT ( 'NONE', #22062 ) ;
#13922 = ORIENTED_EDGE ( 'NONE', *, *, #9504, .F. ) ;
#13923 = CARTESIAN_POINT ( 'NONE',  ( -28.87540678000427619, -6.494748934539263274, 7.799999999999999822 ) ) ;
#13924 = DIRECTION ( 'NONE',  ( 1.000000000000000000, 0.000000000000000000, 6.123233995736764803E-17 ) ) ;
#13925 = EDGE_CURVE ( 'NONE', #2722, #11031, #10187, .T. ) ;
#13926 = VECTOR ( 'NONE', #4415, 1000.000000000000000 ) ;
#13927 = FACE_OUTER_BOUND ( 'NONE', #21232, .T. ) ;
#13928 = AXIS2_PLACEMENT_3D ( 'NONE', #6824, #6375, #10153 ) ;
#13929 = MECHANICAL_DESIGN_GEOMETRIC_PRESENTATION_REPRESENTATION (  '', ( #15719 ), #20737 ) ;
#13930 = FACE_OUTER_BOUND ( 'NONE', #1776, .T. ) ;
#13931 = ORIENTED_EDGE ( 'NONE', *, *, #12682, .T. ) ;
#13932 = FACE_BOUND ( 'NONE', #9635, .T. ) ;
#13933 = ORIENTED_EDGE ( 'NONE', *, *, #9818, .F. ) ;
#13934 = CARTESIAN_POINT ( 'NONE',  ( 30.79999999999999716, -85.00000000000000000, 1.734723475976807094E-15 ) ) ;
#13935 = DIRECTION ( 'NONE',  ( -0.000000000000000000, -0.000000000000000000, -1.000000000000000000 ) ) ;
#13936 = DIRECTION ( 'NONE',  ( 0.000000000000000000, 1.000000000000000000, 0.000000000000000000 ) ) ;
#13937 = ORIENTED_EDGE ( 'NONE', *, *, #250, .T. ) ;
#13938 = DIRECTION ( 'NONE',  ( 1.000000000000000000, -0.000000000000000000, 0.000000000000000000 ) ) ;
#13939 = PLANE ( 'NONE',  #17450 ) ;
#13940 = VECTOR ( 'NONE', #10018, 1000.000000000000000 ) ;
#13941 = EDGE_CURVE ( 'NONE', #5643, #3983, #20384, .T. ) ;
#13942 = TOROIDAL_SURFACE ( 'NONE', #1091, 0.05000000000000000278, 0.05000000000000000278 ) ;
#13943 = DIRECTION ( 'NONE',  ( -0.000000000000000000, -0.000000000000000000, -1.000000000000000000 ) ) ;
#13944 = CARTESIAN_POINT ( 'NONE',  ( -30.79999999999999361, -123.9599366953518711, 0.2999999999999999334 ) ) ;
#13945 = VERTEX_POINT ( 'NONE', #10087 ) ;
#13946 = EDGE_CURVE ( 'NONE', #119, #3262, #5453, .T. ) ;
#13947 = DIRECTION ( 'NONE',  ( 0.000000000000000000, 0.000000000000000000, 1.000000000000000000 ) ) ;
#13948 = VERTEX_POINT ( 'NONE', #1558 ) ;
#13949 = DIRECTION ( 'NONE',  ( 0.000000000000000000, -0.000000000000000000, 1.000000000000000000 ) ) ;
#13950 = FACE_OUTER_BOUND ( 'NONE', #21137, .T. ) ;
#13951 = ORIENTED_EDGE ( 'NONE', *, *, #7051, .T. ) ;
#13952 = ORIENTED_EDGE ( 'NONE', *, *, #16473, .T. ) ;
#13953 = DIRECTION ( 'NONE',  ( -1.000000000000000000, 0.000000000000000000, 0.000000000000000000 ) ) ;
#13954 = ORIENTED_EDGE ( 'NONE', *, *, #14882, .F. ) ;
#13955 = AXIS2_PLACEMENT_3D ( 'NONE', #6256, #14499, #11587 ) ;
#13956 = ORIENTED_EDGE ( 'NONE', *, *, #1016, .F. ) ;
#13957 = EDGE_CURVE ( 'NONE', #1047, #2085, #1497, .T. ) ;
#13958 = ORIENTED_EDGE ( 'NONE', *, *, #3701, .T. ) ;
#13959 = DIRECTION ( 'NONE',  ( -2.107255972849994642E-16, 0.000000000000000000, -1.000000000000000000 ) ) ;
#13960 = CARTESIAN_POINT ( 'NONE',  ( -3.127054932750481964, -32.61873716947361856, 42.50000000000000711 ) ) ;
#13961 = CARTESIAN_POINT ( 'NONE',  ( 1.824728116533979705, 43.26054587065083012, 53.66679706732590915 ) ) ;
#13962 = ADVANCED_FACE ( 'NONE', ( #3257 ), #2408, .F. ) ;
#13963 = AXIS2_PLACEMENT_3D ( 'NONE', #838, #12359, #2201 ) ;
#13964 = AXIS2_PLACEMENT_3D ( 'NONE', #12453, #12658, #2279 ) ;
#13965 = FACE_OUTER_BOUND ( 'NONE', #7696, .T. ) ;
#13966 = VERTEX_POINT ( 'NONE', #11525 ) ;
#13967 = DIRECTION ( 'NONE',  ( 0.000000000000000000, 0.000000000000000000, -1.000000000000000000 ) ) ;
#13968 = AXIS2_PLACEMENT_3D ( 'NONE', #14145, #16043, #2407 ) ;
#13969 = CARTESIAN_POINT ( 'NONE',  ( -33.20000000000000284, 85.00000000000000000, 1.200000000000000178 ) ) ;
#13970 = CARTESIAN_POINT ( 'NONE',  ( -1.724728116533986721, 42.36054587065083155, 49.76679706732591058 ) ) ;
#13971 = ORIENTED_EDGE ( 'NONE', *, *, #3698, .T. ) ;
#13972 = CYLINDRICAL_SURFACE ( 'NONE', #13844, 0.3000000000000003775 ) ;
#13973 = CARTESIAN_POINT ( 'NONE',  ( -14.96174975910705207, 51.83071861726173779, 13.82019355104894309 ) ) ;
#13974 = AXIS2_PLACEMENT_3D ( 'NONE', #11103, #7768, #14571 ) ;
#13975 = VERTEX_POINT ( 'NONE', #11749 ) ;
#13976 = VERTEX_POINT ( 'NONE', #20495 ) ;
#13977 = CARTESIAN_POINT ( 'NONE',  ( 30.79999999999999716, -84.70000000000001705, 1.200000000000004174 ) ) ;
#13978 = CARTESIAN_POINT ( 'NONE',  ( -18.35781278715831633, 0.000000000000000000, 0.000000000000000000 ) ) ;
#13979 = EDGE_CURVE ( 'NONE', #7925, #11776, #18577, .T. ) ;
#13980 = VECTOR ( 'NONE', #5309, 1000.000000000000000 ) ;
#13981 = EDGE_LOOP ( 'NONE', ( #15394, #16158, #14779, #16960 ) ) ;
#13982 = AXIS2_PLACEMENT_3D ( 'NONE', #5312, #10448, #17255 ) ;
#13983 = ORIENTED_EDGE ( 'NONE', *, *, #12644, .F. ) ;
#13984 = LINE ( 'NONE', #14320, #20093 ) ;
#13985 = VERTEX_POINT ( 'NONE', #13649 ) ;
#13986 = ORIENTED_EDGE ( 'NONE', *, *, #18893, .F. ) ;
#13987 = EDGE_CURVE ( 'NONE', #13526, #15347, #11858, .T. ) ;
#13988 = FACE_OUTER_BOUND ( 'NONE', #14985, .T. ) ;
#13989 = ADVANCED_FACE ( 'NONE', ( #13317 ), #5090, .T. ) ;
#13990 = CARTESIAN_POINT ( 'NONE',  ( 31.69597781366222122, 27.99124249474150972, 70.25000000000000000 ) ) ;
#13991 = DIRECTION ( 'NONE',  ( 0.000000000000000000, 0.000000000000000000, 1.000000000000000000 ) ) ;
#13992 = EDGE_CURVE ( 'NONE', #583, #3057, #3809, .T. ) ;
#13993 = B_SPLINE_CURVE_WITH_KNOTS ( 'NONE', 3,
 ( #4509, #11216, #11329, #19503, #4183, #9328, #7656, #11448, #9779, #6318, #18275, #6772, #13118, #8423 ),
 .UNSPECIFIED., .F., .F.,
 ( 4, 2, 2, 2, 2, 2, 4 ),
 ( 0.000000000000000000, 0.0006835338044177908991, 0.001025300706626684722, 0.001196184157731131200, 0.001281625883283354006, 0.001324346746059462589, 0.001367067608835571173 ),
 .UNSPECIFIED. ) ;
#13994 = AXIS2_PLACEMENT_3D ( 'NONE', #500, #13713, #3667 ) ;
#13995 =( LENGTH_UNIT ( ) NAMED_UNIT ( * ) SI_UNIT ( .MILLI., .METRE. ) );
#13996 = VECTOR ( 'NONE', #11297, 1000.000000000000000 ) ;
#13997 = CARTESIAN_POINT ( 'NONE',  ( -31.69597781366222122, 58.94165929845684815, 70.50000000000000000 ) ) ;
#13998 = CIRCLE ( 'NONE', #10457, 0.2999999999999999334 ) ;
#13999 = FACE_OUTER_BOUND ( 'NONE', #53, .T. ) ;
#14000 = CARTESIAN_POINT ( 'NONE',  ( -34.39999999999999858, 84.70000000000001705, 0.3000000000000000444 ) ) ;
#14001 = DIRECTION ( 'NONE',  ( 1.000000000000000000, 0.000000000000000000, 0.000000000000000000 ) ) ;
#14002 = CARTESIAN_POINT ( 'NONE',  ( 34.39999999999998437, -84.70000000000001705, 0.3000000000000042077 ) ) ;
#14003 = ORIENTED_EDGE ( 'NONE', *, *, #4452, .T. ) ;
#14004 = ORIENTED_EDGE ( 'NONE', *, *, #9536, .F. ) ;
#14005 = CARTESIAN_POINT ( 'NONE',  ( -5.428906393579158163, 42.46645089659918426, 67.85468508031152624 ) ) ;
#14006 =( NAMED_UNIT ( * ) PLANE_ANGLE_UNIT ( ) SI_UNIT ( $, .RADIAN. ) );
#14007 = DIRECTION ( 'NONE',  ( 0.000000000000000000, 0.000000000000000000, 1.000000000000000000 ) ) ;
#14008 = EDGE_CURVE ( 'NONE', #18617, #13360, #10103, .T. ) ;
#14009 = EDGE_LOOP ( 'NONE', ( #15918, #17997, #10572, #15639 ) ) ;
#14010 = ORIENTED_EDGE ( 'NONE', *, *, #18839, .T. ) ;
#14011 = AXIS2_PLACEMENT_3D ( 'NONE', #19030, #19131, #3696 ) ;
#14012 = AXIS2_PLACEMENT_3D ( 'NONE', #13022, #21896, #19766 ) ;
#14013 = EDGE_CURVE ( 'NONE', #16038, #124, #7600, .T. ) ;
#14014 = LINE ( 'NONE', #20860, #5630 ) ;
#14015 = EDGE_CURVE ( 'NONE', #381, #4085, #3672, .T. ) ;
#14016 = DIRECTION ( 'NONE',  ( -0.2309407893632117181, 0.9729678061520313781, 0.000000000000000000 ) ) ;
#14017 = ORIENTED_EDGE ( 'NONE', *, *, #7546, .T. ) ;
#14018 = SPHERICAL_SURFACE ( 'NONE', #3230, 0.2500000000000000000 ) ;
#14019 = AXIS2_PLACEMENT_3D ( 'NONE', #22092, #1820, #8658 ) ;
#14020 = EDGE_CURVE ( 'NONE', #6249, #1178, #5274, .T. ) ;
#14021 = DIRECTION ( 'NONE',  ( 0.000000000000000000, 1.000000000000000000, 0.000000000000000000 ) ) ;
#14022 = CARTESIAN_POINT ( 'NONE',  ( 25.37540678000427263, 67.54634676501045476, 7.799999999999999822 ) ) ;
#14023 = DIRECTION ( 'NONE',  ( -0.000000000000000000, 0.000000000000000000, -1.000000000000000000 ) ) ;
#14024 = CARTESIAN_POINT ( 'NONE',  ( 0.000000000000000000, 43.26054587065083012, 51.75876104995654003 ) ) ;
#14025 = CARTESIAN_POINT ( 'NONE',  ( 1.774728116533979438, 42.36054587065083155, 35.80876104995653009 ) ) ;
#14026 = DIRECTION ( 'NONE',  ( -1.000000000000000000, -0.000000000000000000, -0.000000000000000000 ) ) ;
#14027 = ORIENTED_EDGE ( 'NONE', *, *, #9904, .F. ) ;
#14028 = CARTESIAN_POINT ( 'NONE',  ( 1.724728116533978728, 43.31054587065082728, 49.71679706732589921 ) ) ;
#14029 = DIRECTION ( 'NONE',  ( 0.000000000000000000, 0.000000000000000000, 1.000000000000000000 ) ) ;
#14030 = DIRECTION ( 'NONE',  ( 0.000000000000000000, 0.000000000000000000, 1.000000000000000000 ) ) ;
#14031 = ORIENTED_EDGE ( 'NONE', *, *, #21723, .T. ) ;
#14032 = ORIENTED_EDGE ( 'NONE', *, *, #20859, .F. ) ;
#14033 = ORIENTED_EDGE ( 'NONE', *, *, #10842, .F. ) ;
#14034 = DIRECTION ( 'NONE',  ( -0.000000000000000000, -1.000000000000000000, 0.000000000000000000 ) ) ;
#14035 = DIRECTION ( 'NONE',  ( -0.000000000000000000, 1.000000000000000000, 0.000000000000000000 ) ) ;
#14036 = DIRECTION ( 'NONE',  ( 1.000000000000000000, 0.000000000000000000, 0.000000000000000000 ) ) ;
#14037 = ADVANCED_FACE ( 'NONE', ( #10417 ), #17226, .T. ) ;
#14038 = ORIENTED_EDGE ( 'NONE', *, *, #15, .T. ) ;
#14039 = DIRECTION ( 'NONE',  ( 1.000000000000000000, 0.000000000000000000, 0.000000000000000000 ) ) ;
#14040 = EDGE_CURVE ( 'NONE', #15569, #8198, #658, .T. ) ;
#14041 = ORIENTED_EDGE ( 'NONE', *, *, #20434, .F. ) ;
#14042 = DIRECTION ( 'NONE',  ( 0.000000000000000000, -1.000000000000000000, 0.000000000000000000 ) ) ;
#14043 = VERTEX_POINT ( 'NONE', #15533 ) ;
#14044 = CARTESIAN_POINT ( 'NONE',  ( -1.774728116533986766, 43.31054587065082728, 49.66679706732590915 ) ) ;
#14045 = FACE_OUTER_BOUND ( 'NONE', #4822, .T. ) ;
#14046 = CARTESIAN_POINT ( 'NONE',  ( 17.45292532278785913, -50.11873716947361856, 68.00000000000000000 ) ) ;
#14047 = DIRECTION ( 'NONE',  ( -1.000000000000000000, -3.052134192567367925E-16, 0.000000000000000000 ) ) ;
#14048 = ORIENTED_EDGE ( 'NONE', *, *, #15691, .F. ) ;
#14049 = CARTESIAN_POINT ( 'NONE',  ( -27.37540678000427619, 7.754037881813018962E-15, 42.50000000000000000 ) ) ;
#14050 = EDGE_CURVE ( 'NONE', #14759, #16038, #2231, .T. ) ;
#14051 = CARTESIAN_POINT ( 'NONE',  ( -1.824728116533986810, 43.31054587065082728, 39.70876104995653577 ) ) ;
#14052 = DIRECTION ( 'NONE',  ( 0.000000000000000000, 0.000000000000000000, 1.000000000000000000 ) ) ;
#14053 = LINE ( 'NONE', #9253, #20336 ) ;
#14054 = VERTEX_POINT ( 'NONE', #10745 ) ;
#14055 = DIRECTION ( 'NONE',  ( -0.000000000000000000, 0.000000000000000000, 1.000000000000000000 ) ) ;
#14056 = ORIENTED_EDGE ( 'NONE', *, *, #18856, .T. ) ;
#14057 = DIRECTION ( 'NONE',  ( 1.000000000000000000, 0.000000000000000000, 0.000000000000000000 ) ) ;
#14058 = DIRECTION ( 'NONE',  ( -0.000000000000000000, -0.000000000000000000, -1.000000000000000000 ) ) ;
#14059 = COLOUR_RGB ( '', 0.09019608, 0.27058824, 0.51372549) ;
#14060 = ORIENTED_EDGE ( 'NONE', *, *, #110, .T. ) ;
#14061 = ORIENTED_EDGE ( 'NONE', *, *, #14541, .T. ) ;
#14062 = DIRECTION ( 'NONE',  ( 0.000000000000000000, 0.000000000000000000, 1.000000000000000000 ) ) ;
#14063 = DIRECTION ( 'NONE',  ( -0.000000000000000000, 1.000000000000000000, -0.000000000000000000 ) ) ;
#14064 = ORIENTED_EDGE ( 'NONE', *, *, #19707, .T. ) ;
#14065 = EDGE_CURVE ( 'NONE', #2269, #6210, #10456, .T. ) ;
#14066 = VECTOR ( 'NONE', #5364, 1000.000000000000000 ) ;
#14067 = ADVANCED_FACE ( 'NONE', ( #12394, #2229, #9060 ), #12279, .F. ) ;
#14068 = ORIENTED_EDGE ( 'NONE', *, *, #5277, .F. ) ;
#14069 = EDGE_CURVE ( 'NONE', #11863, #8916, #10844, .T. ) ;
#14070 = CARTESIAN_POINT ( 'NONE',  ( -31.50000000000002132, -71.70000000000001705, 3.500000000000000000 ) ) ;
#14071 = DIRECTION ( 'NONE',  ( 0.000000000000000000, 0.000000000000000000, 1.000000000000000000 ) ) ;
#14072 = CIRCLE ( 'NONE', #19089, 0.2999999999999999334 ) ;
#14073 = CIRCLE ( 'NONE', #492, 0.04999999999999991257 ) ;
#14074 = FACE_OUTER_BOUND ( 'NONE', #10095, .T. ) ;
#14075 = DIRECTION ( 'NONE',  ( 0.000000000000000000, -1.000000000000000000, 0.000000000000000000 ) ) ;
#14076 = DIRECTION ( 'NONE',  ( 0.000000000000000000, 0.000000000000000000, -1.000000000000000000 ) ) ;
#14077 = ORIENTED_EDGE ( 'NONE', *, *, #17150, .F. ) ;
#14078 = DIRECTION ( 'NONE',  ( -0.000000000000000000, -0.000000000000000000, -1.000000000000000000 ) ) ;
#14079 = DIRECTION ( 'NONE',  ( 1.000000000000000000, 0.000000000000000000, 0.000000000000000000 ) ) ;
#14080 = DIRECTION ( 'NONE',  ( 1.000000000000000000, 0.000000000000000000, 0.000000000000000000 ) ) ;
#14081 = ORIENTED_EDGE ( 'NONE', *, *, #11469, .F. ) ;
#14082 = ORIENTED_EDGE ( 'NONE', *, *, #10824, .F. ) ;
#14083 = EDGE_LOOP ( 'NONE', ( #9774, #8619, #554, #14647, #9270, #18500, #10043, #13937, #6421, #15069 ) ) ;
#14084 = EDGE_CURVE ( 'NONE', #4893, #5864, #20713, .T. ) ;
#14085 = ORIENTED_EDGE ( 'NONE', *, *, #20359, .F. ) ;
#14086 = ORIENTED_EDGE ( 'NONE', *, *, #14623, .T. ) ;
#14087 = CARTESIAN_POINT ( 'NONE',  ( 23.02398829872513986, -2.928406208502775776, 13.54172988673462896 ) ) ;
#14088 = ORIENTED_EDGE ( 'NONE', *, *, #14704, .F. ) ;
#14089 = ORIENTED_EDGE ( 'NONE', *, *, #20702, .F. ) ;
#14090 = CARTESIAN_POINT ( 'NONE',  ( 17.95292532278785913, -50.11873716947361856, 14.00000000000000000 ) ) ;
#14091 = CARTESIAN_POINT ( 'NONE',  ( 29.05186365738250842, 0.05288320938007240457, -150.0833101980363722 ) ) ;
#14092 = DIRECTION ( 'NONE',  ( 0.5176069476490314791, -0.8556185176499236933, 0.000000000000000000 ) ) ;
#14093 = CIRCLE ( 'NONE', #5197, 0.3000000000000016542 ) ;
#14094 = VECTOR ( 'NONE', #2481, 1000.000000000000000 ) ;
#14095 = DIRECTION ( 'NONE',  ( -2.105859220307292343E-16, 1.000000000000000000, 0.000000000000000000 ) ) ;
#14096 = DIRECTION ( 'NONE',  ( -1.000000000000000000, 0.000000000000000000, -0.000000000000000000 ) ) ;
#14097 = CYLINDRICAL_SURFACE ( 'NONE', #17585, 0.2999999999999999889 ) ;
#14098 = CARTESIAN_POINT ( 'NONE',  ( -9.178906393579158163, 42.46645089659918426, 70.88527860057354246 ) ) ;
#14099 = DIRECTION ( 'NONE',  ( 0.000000000000000000, 0.000000000000000000, -1.000000000000000000 ) ) ;
#14100 = DIRECTION ( 'NONE',  ( -1.000000000000000000, -0.000000000000000000, -0.000000000000000000 ) ) ;
#14101 = ORIENTED_EDGE ( 'NONE', *, *, #1281, .F. ) ;
#14102 = ORIENTED_EDGE ( 'NONE', *, *, #16871, .T. ) ;
#14103 = CARTESIAN_POINT ( 'NONE',  ( 34.99999999999999289, 85.00000000000000000, 79.39999999999999147 ) ) ;
#14104 = EDGE_CURVE ( 'NONE', #1590, #20541, #4033, .T. ) ;
#14105 = SURFACE_SIDE_STYLE ('',( #7313 ) ) ;
#14106 = DIRECTION ( 'NONE',  ( 1.000000000000000000, 0.000000000000000000, 0.000000000000000000 ) ) ;
#14107 = VERTEX_POINT ( 'NONE', #13970 ) ;
#14108 = EDGE_CURVE ( 'NONE', #6971, #13921, #15091, .T. ) ;
#14109 = EDGE_LOOP ( 'NONE', ( #11308, #3934, #93, #4535 ) ) ;
#14110 = CIRCLE ( 'NONE', #20204, 1.000000000000000888 ) ;
#14111 = AXIS2_PLACEMENT_3D ( 'NONE', #2425, #16506, #12922 ) ;
#14112 = ORIENTED_EDGE ( 'NONE', *, *, #15398, .T. ) ;
#14113 = DIRECTION ( 'NONE',  ( 0.000000000000000000, 0.000000000000000000, 1.000000000000000000 ) ) ;
#14114 = DIRECTION ( 'NONE',  ( -0.000000000000000000, -0.000000000000000000, 1.000000000000000000 ) ) ;
#14115 = AXIS2_PLACEMENT_3D ( 'NONE', #2675, #13499, #5012 ) ;
#14116 = ORIENTED_EDGE ( 'NONE', *, *, #17949, .F. ) ;
#14117 = CARTESIAN_POINT ( 'NONE',  ( -29.69597781366221767, 58.69165929845684104, 70.50000000000000000 ) ) ;
#14118 = CARTESIAN_POINT ( 'NONE',  ( 15.95292532278785913, -52.39333383871510108, 13.79999999999999893 ) ) ;
#14119 = EDGE_CURVE ( 'NONE', #299, #6925, #5472, .T. ) ;
#14120 = CARTESIAN_POINT ( 'NONE',  ( 27.37540678000427974, -5.683640910026986681, 13.79999999999999893 ) ) ;
#14121 = DIRECTION ( 'NONE',  ( -0.000000000000000000, -0.000000000000000000, -1.000000000000000000 ) ) ;
#14122 = DIRECTION ( 'NONE',  ( 0.000000000000000000, 0.000000000000000000, 1.000000000000000000 ) ) ;
#14123 = CARTESIAN_POINT ( 'NONE',  ( -3.127054932750481964, 32.11873716947361856, 109.6002446535588319 ) ) ;
#14124 = CIRCLE ( 'NONE', #20596, 0.2999999999999999334 ) ;
#14125 = CIRCLE ( 'NONE', #20939, 0.2999999999999999334 ) ;
#14126 = AXIS2_PLACEMENT_3D ( 'NONE', #17095, #18767, #16970 ) ;
#14127 = VERTEX_POINT ( 'NONE', #10521 ) ;
#14128 = CARTESIAN_POINT ( 'NONE',  ( 29.37540678000427619, 6.000000000000000000, 3.799999999999999822 ) ) ;
#14129 = DIRECTION ( 'NONE',  ( 0.000000000000000000, -0.000000000000000000, -1.000000000000000000 ) ) ;
#14130 = DIRECTION ( 'NONE',  ( 0.000000000000000000, 1.000000000000000000, 0.000000000000000000 ) ) ;
#14131 = ORIENTED_EDGE ( 'NONE', *, *, #1624, .T. ) ;
#14132 = ORIENTED_EDGE ( 'NONE', *, *, #4055, .T. ) ;
#14133 = ORIENTED_EDGE ( 'NONE', *, *, #13599, .F. ) ;
#14134 = FACE_OUTER_BOUND ( 'NONE', #13101, .T. ) ;
#14135 = CARTESIAN_POINT ( 'NONE',  ( -17.92752199202934094, -38.74634676501045760, 13.79999999999999893 ) ) ;
#14136 = EDGE_CURVE ( 'NONE', #183, #12999, #531, .T. ) ;
#14137 = ORIENTED_EDGE ( 'NONE', *, *, #13873, .F. ) ;
#14138 = EDGE_CURVE ( 'NONE', #2663, #12289, #2120, .T. ) ;
#14139 = AXIS2_PLACEMENT_3D ( 'NONE', #19151, #7300, #14092 ) ;
#14140 = VECTOR ( 'NONE', #3905, 1000.000000000000000 ) ;
#14141 = DIRECTION ( 'NONE',  ( -1.000000000000000000, 0.000000000000000000, 0.000000000000000000 ) ) ;
#14142 = CIRCLE ( 'NONE', #19888, 0.2999999999999947153 ) ;
#14143 = ADVANCED_FACE ( 'NONE', ( #5833 ), #7711, .T. ) ;
#14144 = ORIENTED_EDGE ( 'NONE', *, *, #3078, .F. ) ;
#14145 = CARTESIAN_POINT ( 'NONE',  ( -10.22290649399595353, 43.00645089659918341, 68.06527860057354928 ) ) ;
#14146 = AXIS2_PLACEMENT_3D ( 'NONE', #6434, #1142, #21422 ) ;
#14147 = CARTESIAN_POINT ( 'NONE',  ( -25.37540678000427263, 67.24634676501045760, 7.799999999999999822 ) ) ;
#14148 = EDGE_LOOP ( 'NONE', ( #16815, #18719, #15458, #17510 ) ) ;
#14149 = DIRECTION ( 'NONE',  ( 0.000000000000000000, 0.000000000000000000, 1.000000000000000000 ) ) ;
#14150 = CARTESIAN_POINT ( 'NONE',  ( -26.56227312273159313, -9.958410664601842655, 42.50000000000000000 ) ) ;
#14151 = FACE_OUTER_BOUND ( 'NONE', #13267, .T. ) ;
#14152 = CARTESIAN_POINT ( 'NONE',  ( 25.37540678000427263, 69.04634676501045476, 3.799999999999999822 ) ) ;
#14153 = ORIENTED_EDGE ( 'NONE', *, *, #2625, .T. ) ;
#14154 = FACE_OUTER_BOUND ( 'NONE', #13981, .T. ) ;
#14155 = LINE ( 'NONE', #19102, #20318 ) ;
#14156 = ADVANCED_FACE ( 'NONE', ( #19916 ), #1102, .T. ) ;
#14157 = CARTESIAN_POINT ( 'NONE',  ( -30.67540678000427690, -6.000000000000000000, 3.500000000000000000 ) ) ;
#14158 = CARTESIAN_POINT ( 'NONE',  ( -23.04273156199908357, -2.261510999192740901, 7.500000000000000000 ) ) ;
#14159 = VERTEX_POINT ( 'NONE', #2784 ) ;
#14160 = CIRCLE ( 'NONE', #6328, 0.2500000000000002220 ) ;
#14161 = AXIS2_PLACEMENT_3D ( 'NONE', #1078, #7591, #12814 ) ;
#14162 = FACE_OUTER_BOUND ( 'NONE', #16521, .T. ) ;
#14163 = TOROIDAL_SURFACE ( 'NONE', #2734, 0.7000000000000000666, 0.2999999999999999889 ) ;
#14164 = ORIENTED_EDGE ( 'NONE', *, *, #5787, .F. ) ;
#14165 = CARTESIAN_POINT ( 'NONE',  ( 4.127054932750481520, -32.93424481021354921, 68.00000000000000000 ) ) ;
#14166 = FACE_OUTER_BOUND ( 'NONE', #1395, .T. ) ;
#14167 = EDGE_LOOP ( 'NONE', ( #9179, #6988, #7242, #7178 ) ) ;
#14168 = AXIS2_PLACEMENT_3D ( 'NONE', #20268, #14885, #20156 ) ;
#14169 = VERTEX_POINT ( 'NONE', #12614 ) ;
#14170 = CARTESIAN_POINT ( 'NONE',  ( 13.37248138918699425, 42.46645089659917716, 70.50000000000000000 ) ) ;
#14171 = ADVANCED_FACE ( 'NONE', ( #19799 ), #16534, .T. ) ;
#14172 = ORIENTED_EDGE ( 'NONE', *, *, #11157, .F. ) ;
#14173 = ADVANCED_FACE ( 'NONE', ( #11398 ), #14751, .T. ) ;
#14174 = AXIS2_PLACEMENT_3D ( 'NONE', #16125, #2493, #2946 ) ;
#14175 = EDGE_LOOP ( 'NONE', ( #16728, #19618, #4462, #12221 ) ) ;
#14176 = AXIS2_PLACEMENT_3D ( 'NONE', #1944, #67, #14030 ) ;
#14177 = AXIS2_PLACEMENT_3D ( 'NONE', #1427, #20230, #11719 ) ;
#14178 = VERTEX_POINT ( 'NONE', #2565 ) ;
#14179 = DIRECTION ( 'NONE',  ( -1.000000000000000000, 0.000000000000000000, 0.000000000000000000 ) ) ;
#14180 = VECTOR ( 'NONE', #2513, 1000.000000000000000 ) ;
#14181 = CIRCLE ( 'NONE', #5287, 0.2999999999999999334 ) ;
#14182 = DIRECTION ( 'NONE',  ( 0.000000000000000000, 0.000000000000000000, -1.000000000000000000 ) ) ;
#14183 = DIRECTION ( 'NONE',  ( -0.000000000000000000, 0.000000000000000000, 1.000000000000000000 ) ) ;
#14184 = DIRECTION ( 'NONE',  ( 0.000000000000000000, 1.000000000000000000, 0.000000000000000000 ) ) ;
#14185 = ORIENTED_EDGE ( 'NONE', *, *, #11025, .T. ) ;
#14186 = CARTESIAN_POINT ( 'NONE',  ( -14.96174975910705207, 51.86873716947361856, 14.00000000000000000 ) ) ;
#14187 = EDGE_CURVE ( 'NONE', #14272, #6455, #1512, .T. ) ;
#14188 = CARTESIAN_POINT ( 'NONE',  ( -27.37540678000427974, -5.683640910026986681, 42.50000000000000000 ) ) ;
#14189 = EDGE_CURVE ( 'NONE', #4651, #7158, #7968, .T. ) ;
#14190 = DIRECTION ( 'NONE',  ( 1.000000000000000000, 0.000000000000000000, 0.000000000000000000 ) ) ;
#14191 = VECTOR ( 'NONE', #21036, 1000.000000000000000 ) ;
#14192 = AXIS2_PLACEMENT_3D ( 'NONE', #7937, #4348, #6151 ) ;
#14193 = TOROIDAL_SURFACE ( 'NONE', #10291, 0.05000000000000000278, 0.05000000000000000278 ) ;
#14194 = ORIENTED_EDGE ( 'NONE', *, *, #2127, .F. ) ;
#14195 = DIRECTION ( 'NONE',  ( 0.000000000000000000, 0.000000000000000000, 1.000000000000000000 ) ) ;
#14196 = ORIENTED_EDGE ( 'NONE', *, *, #14758, .T. ) ;
#14197 = AXIS2_PLACEMENT_3D ( 'NONE', #17724, #17519, #9237 ) ;
#14198 = ORIENTED_EDGE ( 'NONE', *, *, #21540, .F. ) ;
#14199 = CIRCLE ( 'NONE', #14547, 5.300000000000006040 ) ;
#14200 = CARTESIAN_POINT ( 'NONE',  ( -1.724728116533986721, 43.26054587065083012, 47.80876104995653719 ) ) ;
#14201 = CIRCLE ( 'NONE', #11347, 4.351418481279133665 ) ;
#14203 = ADVANCED_FACE ( 'NONE', ( #5930 ), #14515, .F. ) ;
#14202 = APPLICATION_PROTOCOL_DEFINITION ( 'draft international standard', 'automotive_design', 1998, #14566 ) ;
#14204 = ORIENTED_EDGE ( 'NONE', *, *, #20302, .F. ) ;
#14205 = ORIENTED_EDGE ( 'NONE', *, *, #14344, .T. ) ;
#14206 = CARTESIAN_POINT ( 'NONE',  ( 23.32398829872514057, -3.528912754968634324, 13.50000000000000000 ) ) ;
#14207 = ORIENTED_EDGE ( 'NONE', *, *, #17932, .T. ) ;
#14208 = CARTESIAN_POINT ( 'NONE',  ( -0.000000000000000000, 51.61873716947361856, 68.50000000000000000 ) ) ;
#14209 = CIRCLE ( 'NONE', #17083, 0.5000000000000004441 ) ;
#14210 = CIRCLE ( 'NONE', #12068, 0.5000000000000004441 ) ;
#14211 = AXIS2_PLACEMENT_3D ( 'NONE', #1436, #21931, #6608 ) ;
#14212 = ORIENTED_EDGE ( 'NONE', *, *, #14899, .T. ) ;
#14213 = DIRECTION ( 'NONE',  ( -1.000000000000000000, 0.000000000000000000, -6.123233995736764803E-17 ) ) ;
#14214 = CARTESIAN_POINT ( 'NONE',  ( 1.724728116533979616, 43.26054587065083012, 47.70876104995654288 ) ) ;
#14215 = CARTESIAN_POINT ( 'NONE',  ( 30.37540678000427619, 6.000000000000000000, 3.799999999999999822 ) ) ;
#14216 = AXIS2_PLACEMENT_3D ( 'NONE', #9849, #3135, #16656 ) ;
#14217 = AXIS2_PLACEMENT_3D ( 'NONE', #14668, #2826, #17916 ) ;
#14218 = DIRECTION ( 'NONE',  ( -4.336808689941893885E-15, 0.000000000000000000, 1.000000000000000000 ) ) ;
#14219 = AXIS2_PLACEMENT_3D ( 'NONE', #6929, #20561, #5239 ) ;
#14220 = EDGE_CURVE ( 'NONE', #21877, #17488, #4578, .T. ) ;
#14221 = CARTESIAN_POINT ( 'NONE',  ( -23.02398829872513986, 2.501891433834999567, 13.57888791970315445 ) ) ;
#14222 = FACE_OUTER_BOUND ( 'NONE', #15987, .T. ) ;
#14223 = EDGE_CURVE ( 'NONE', #5602, #9461, #16880, .T. ) ;
#14224 = DIRECTION ( 'NONE',  ( -1.000000000000000000, 0.000000000000000000, 0.000000000000000000 ) ) ;
#14225 = VECTOR ( 'NONE', #19173, 1000.000000000000000 ) ;
#14226 = TOROIDAL_SURFACE ( 'NONE', #18510, 5.193574995607837863, 1.000000000000000000 ) ;
#14227 = VERTEX_POINT ( 'NONE', #4360 ) ;
#14228 = EDGE_LOOP ( 'NONE', ( #1203, #15322, #17292, #9632 ) ) ;
#14229 = DIRECTION ( 'NONE',  ( 2.107255972849994642E-16, -0.000000000000000000, 1.000000000000000000 ) ) ;
#14230 =( NAMED_UNIT ( * ) SI_UNIT ( $, .STERADIAN. ) SOLID_ANGLE_UNIT ( ) );
#14231 = ORIENTED_EDGE ( 'NONE', *, *, #11652, .T. ) ;
#14232 = AXIS2_PLACEMENT_3D ( 'NONE', #9486, #16294, #978 ) ;
#14233 = ORIENTED_EDGE ( 'NONE', *, *, #1885, .F. ) ;
#14234 = AXIS2_PLACEMENT_3D ( 'NONE', #3732, #15473, #3517 ) ;
#14235 = VECTOR ( 'NONE', #11636, 1000.000000000000000 ) ;
#14236 = ORIENTED_EDGE ( 'NONE', *, *, #7174, .T. ) ;
#14237 = ADVANCED_FACE ( 'NONE', ( #6270 ), #4129, .F. ) ;
#14238 = DIRECTION ( 'NONE',  ( -1.000000000000000000, 0.000000000000000000, 0.000000000000000000 ) ) ;
#14239 = AXIS2_PLACEMENT_3D ( 'NONE', #7036, #18773, #20571 ) ;
#14240 = DIRECTION ( 'NONE',  ( -1.000000000000000000, 0.000000000000000000, 0.000000000000000000 ) ) ;
#14241 = VERTEX_POINT ( 'NONE', #16086 ) ;
#14242 = CARTESIAN_POINT ( 'NONE',  ( 15.95292532278785913, -34.11873716947361856, 68.50000000000000000 ) ) ;
#14243 = CARTESIAN_POINT ( 'NONE',  ( -21.67365502786443088, 45.72430987248279166, 68.50000000000000000 ) ) ;
#14244 = EDGE_CURVE ( 'NONE', #13377, #11313, #15797, .T. ) ;
#14245 = EDGE_CURVE ( 'NONE', #11756, #9769, #985, .T. ) ;
#14246 = DIRECTION ( 'NONE',  ( -0.000000000000000000, -0.000000000000000000, -1.000000000000000000 ) ) ;
#14247 = VECTOR ( 'NONE', #5898, 1000.000000000000000 ) ;
#14248 = CARTESIAN_POINT ( 'NONE',  ( 14.98281217233416562, 51.83338592095527275, 13.50000000000000000 ) ) ;
#14249 = DIRECTION ( 'NONE',  ( 0.000000000000000000, 0.000000000000000000, -1.000000000000000000 ) ) ;
#14250 = DIRECTION ( 'NONE',  ( 1.000000000000000000, 0.000000000000000000, 0.000000000000000000 ) ) ;
#14251 = VECTOR ( 'NONE', #766, 1000.000000000000000 ) ;
#14252 = DIRECTION ( 'NONE',  ( 1.000000000000000000, 0.000000000000000000, 0.000000000000000000 ) ) ;
#14253 = CARTESIAN_POINT ( 'NONE',  ( 1.724728116533979616, 42.36054587065083155, 47.80876104995653719 ) ) ;
#14254 = DIRECTION ( 'NONE',  ( 0.000000000000000000, 0.000000000000000000, 1.000000000000000000 ) ) ;
#14255 = ORIENTED_EDGE ( 'NONE', *, *, #21452, .F. ) ;
#14256 = EDGE_LOOP ( 'NONE', ( #18407, #13782, #5027, #15741 ) ) ;
#14257 = ORIENTED_EDGE ( 'NONE', *, *, #10455, .T. ) ;
#14258 = LINE ( 'NONE', #16036, #18870 ) ;
#14259 = DIRECTION ( 'NONE',  ( 0.000000000000000000, 0.000000000000000000, 1.000000000000000000 ) ) ;
#14260 = ORIENTED_EDGE ( 'NONE', *, *, #19862, .F. ) ;
#14261 = CYLINDRICAL_SURFACE ( 'NONE', #22085, 0.3000000000000003775 ) ;
#14262 = ADVANCED_FACE ( 'NONE', ( #14637 ), #21184, .T. ) ;
#14263 = VECTOR ( 'NONE', #14998, 1000.000000000000000 ) ;
#14264 = EDGE_LOOP ( 'NONE', ( #10141, #6353, #11944 ) ) ;
#14265 = CARTESIAN_POINT ( 'NONE',  ( -9.641460742840918030, -32.11873716947361856, 42.50000000000000711 ) ) ;
#14266 = CARTESIAN_POINT ( 'NONE',  ( -1.724728116533986721, 43.31054587065082728, 43.75876104995654003 ) ) ;
#14267 = ORIENTED_EDGE ( 'NONE', *, *, #13236, .T. ) ;
#14268 = LINE ( 'NONE', #21450, #7443 ) ;
#14269 = CARTESIAN_POINT ( 'NONE',  ( -9.178906393579161715, 42.46645089659918426, 61.53912392244307483 ) ) ;
#14270 = DIRECTION ( 'NONE',  ( 0.000000000000000000, 0.000000000000000000, 1.000000000000000000 ) ) ;
#14271 = FACE_OUTER_BOUND ( 'NONE', #413, .T. ) ;
#14272 = VERTEX_POINT ( 'NONE', #6165 ) ;
#14273 = FACE_OUTER_BOUND ( 'NONE', #16117, .T. ) ;
#14274 = DIRECTION ( 'NONE',  ( -0.000000000000000000, -0.000000000000000000, -1.000000000000000000 ) ) ;
#14275 = EDGE_CURVE ( 'NONE', #6455, #14043, #8050, .T. ) ;
#14276 = EDGE_CURVE ( 'NONE', #4860, #421, #2906, .T. ) ;
#14277 = DIRECTION ( 'NONE',  ( 0.000000000000000000, 0.000000000000000000, 1.000000000000000000 ) ) ;
#14278 = CARTESIAN_POINT ( 'NONE',  ( 31.50000000000002132, -71.00000000000001421, 3.200000000000000178 ) ) ;
#14279 = VERTEX_POINT ( 'NONE', #13187 ) ;
#14280 = DIRECTION ( 'NONE',  ( 0.000000000000000000, 0.000000000000000000, 1.000000000000000000 ) ) ;
#14281 = ORIENTED_EDGE ( 'NONE', *, *, #371, .T. ) ;
#14282 = CIRCLE ( 'NONE', #11425, 0.05000000000000143219 ) ;
#14283 = CIRCLE ( 'NONE', #17839, 0.3000000000000003775 ) ;
#14284 = DIRECTION ( 'NONE',  ( 1.000000000000000000, 0.000000000000000000, 0.000000000000000000 ) ) ;
#14285 = AXIS2_PLACEMENT_3D ( 'NONE', #12459, #15921, #5785 ) ;
#14286 = FACE_OUTER_BOUND ( 'NONE', #5566, .T. ) ;
#14287 = VERTEX_POINT ( 'NONE', #7010 ) ;
#14288 = ORIENTED_EDGE ( 'NONE', *, *, #20383, .F. ) ;
#14289 = CARTESIAN_POINT ( 'NONE',  ( -9.141460742840918030, 32.93424481021354921, 42.50000000000000000 ) ) ;
#14290 = CARTESIAN_POINT ( 'NONE',  ( 0.000000000000000000, -4.700000000000000178, 3.799999999999999822 ) ) ;
#14291 = ORIENTED_EDGE ( 'NONE', *, *, #20614, .F. ) ;
#14292 = EDGE_CURVE ( 'NONE', #19849, #15889, #5443, .T. ) ;
#14293 = VERTEX_POINT ( 'NONE', #3648 ) ;
#14294 = CIRCLE ( 'NONE', #10746, 0.05000000000000143219 ) ;
#14295 = EDGE_LOOP ( 'NONE', ( #776, #4516, #1208, #11472 ) ) ;
#14296 = LINE ( 'NONE', #9052, #5297 ) ;
#14297 = AXIS2_PLACEMENT_3D ( 'NONE', #17701, #3739, #2270 ) ;
#14298 = CARTESIAN_POINT ( 'NONE',  ( -15.95292532278785913, -34.11873716947361856, 109.6002446535588319 ) ) ;
#14299 = LINE ( 'NONE', #18919, #10652 ) ;
#14300 = EDGE_CURVE ( 'NONE', #12849, #15983, #5341, .T. ) ;
#14301 = ADVANCED_FACE ( 'NONE', ( #13918 ), #20767, .T. ) ;
#14302 = CARTESIAN_POINT ( 'NONE',  ( -27.37540678000427974, -10.94079601157914716, 13.79999999999999893 ) ) ;
#14303 = ORIENTED_EDGE ( 'NONE', *, *, #1782, .F. ) ;
#14304 = CARTESIAN_POINT ( 'NONE',  ( -1.724728116533986721, 43.31054587065082728, 43.75876104995654003 ) ) ;
#14305 = EDGE_CURVE ( 'NONE', #5089, #21686, #389, .T. ) ;
#14306 = DIRECTION ( 'NONE',  ( 0.000000000000000000, 0.000000000000000000, 1.000000000000000000 ) ) ;
#14307 = CARTESIAN_POINT ( 'NONE',  ( 1.774728116533979883, 42.36054587065083155, 53.66679706732590915 ) ) ;
#14308 = VECTOR ( 'NONE', #16606, 1000.000000000000000 ) ;
#14309 = ORIENTED_EDGE ( 'NONE', *, *, #4982, .F. ) ;
#14310 = CARTESIAN_POINT ( 'NONE',  ( -1.724728116533986721, 42.36054587065083155, 29.66679706732590560 ) ) ;
#14311 = CIRCLE ( 'NONE', #20404, 0.2999999999999999334 ) ;
#14312 = ORIENTED_EDGE ( 'NONE', *, *, #18700, .F. ) ;
#14313 = ORIENTED_EDGE ( 'NONE', *, *, #17047, .T. ) ;
#14314 = VERTEX_POINT ( 'NONE', #4695 ) ;
#14315 = CYLINDRICAL_SURFACE ( 'NONE', #21050, 0.2999999999999999334 ) ;
#14316 = ITEM_DEFINED_TRANSFORMATION ( 'NONE', 'NONE', #10870,  #17493 ) ;
#14317 = ORIENTED_EDGE ( 'NONE', *, *, #9755, .T. ) ;
#14318 = ORIENTED_EDGE ( 'NONE', *, *, #19445, .F. ) ;
#14319 = EDGE_CURVE ( 'NONE', #5463, #12408, #9326, .T. ) ;
#14320 = CARTESIAN_POINT ( 'NONE',  ( 15.95292532278785913, 32.61873716947361856, 68.50000000000000000 ) ) ;
#14321 = ORIENTED_EDGE ( 'NONE', *, *, #21733, .T. ) ;
#14322 = CARTESIAN_POINT ( 'NONE',  ( 1.724728116533979616, 43.26054587065083012, 45.76679706732590347 ) ) ;
#14323 = ORIENTED_EDGE ( 'NONE', *, *, #14244, .T. ) ;
#14324 = DIRECTION ( 'NONE',  ( 1.000000000000000000, -0.000000000000000000, -0.000000000000000000 ) ) ;
#14325 = DIRECTION ( 'NONE',  ( 0.000000000000000000, 0.000000000000000000, 1.000000000000000000 ) ) ;
#14326 = DIRECTION ( 'NONE',  ( -0.000000000000000000, -1.000000000000000000, -0.000000000000000000 ) ) ;
#14327 = VECTOR ( 'NONE', #8392, 1000.000000000000000 ) ;
#14328 = EDGE_CURVE ( 'NONE', #4058, #15046, #12535, .T. ) ;
#14329 = CARTESIAN_POINT ( 'NONE',  ( -23.04273161205373910, 2.261511134070790074, 13.23413512703648820 ) ) ;
#14330 = AXIS2_PLACEMENT_3D ( 'NONE', #702, #16022, #7117 ) ;
#14331 = FACE_OUTER_BOUND ( 'NONE', #9335, .T. ) ;
#14332 = PLANE ( 'NONE',  #21986 ) ;
#14333 = CARTESIAN_POINT ( 'NONE',  ( -10.48680304830625154, -2.489116863435002713, 68.25000000000000000 ) ) ;
#14334 = AXIS2_PLACEMENT_3D ( 'NONE', #13117, #9676, #917 ) ;
#14335 = DIRECTION ( 'NONE',  ( 0.000000000000000000, 0.000000000000000000, -1.000000000000000000 ) ) ;
#14336 = CIRCLE ( 'NONE', #9716, 2.767785046117004377 ) ;
#14337 = ORIENTED_EDGE ( 'NONE', *, *, #16756, .F. ) ;
#14338 = ORIENTED_EDGE ( 'NONE', *, *, #12206, .F. ) ;
#14339 = FACE_OUTER_BOUND ( 'NONE', #14435, .T. ) ;
#14340 =( NAMED_UNIT ( * ) SI_UNIT ( $, .STERADIAN. ) SOLID_ANGLE_UNIT ( ) );
#14341 = ORIENTED_EDGE ( 'NONE', *, *, #6545, .F. ) ;
#14342 = EDGE_LOOP ( 'NONE', ( #3166, #7481, #11532, #4062 ) ) ;
#14343 = EDGE_CURVE ( 'NONE', #9447, #13326, #1745, .T. ) ;
#14344 = EDGE_CURVE ( 'NONE', #5463, #11579, #11486, .T. ) ;
#14345 = AXIS2_PLACEMENT_3D ( 'NONE', #2593, #8073, #17802 ) ;
#14346 = CARTESIAN_POINT ( 'NONE',  ( 15.21174975910707161, -51.61873716947361856, 68.25000000000000000 ) ) ;
#14347 = AXIS2_PLACEMENT_3D ( 'NONE', #9182, #15874, #8857 ) ;
#14348 = VECTOR ( 'NONE', #2612, 1000.000000000000000 ) ;
#14349 = FACE_OUTER_BOUND ( 'NONE', #4735, .T. ) ;
#14350 = ORIENTED_EDGE ( 'NONE', *, *, #876, .F. ) ;
#14351 = CARTESIAN_POINT ( 'NONE',  ( -23.02398829872513986, 2.157133568460765538, 42.50000000000000000 ) ) ;
#14352 = DIRECTION ( 'NONE',  ( 0.000000000000000000, 0.000000000000000000, 1.000000000000000000 ) ) ;
#14353 = CARTESIAN_POINT ( 'NONE',  ( 18.22752199202934520, -50.11873716947361856, 13.79999999999999716 ) ) ;
#14354 = CARTESIAN_POINT ( 'NONE',  ( -23.02398829872514341, 2.624937972534823860, 13.63083126556637126 ) ) ;
#14355 = ORIENTED_EDGE ( 'NONE', *, *, #572, .T. ) ;
#14356 = CARTESIAN_POINT ( 'NONE',  ( 28.87540678000428329, -6.494748934539265051, 13.24746166461178554 ) ) ;
#14357 = CARTESIAN_POINT ( 'NONE',  ( -23.37634868863050386, 45.32016349109721176, 13.49999999999999822 ) ) ;
#14358 = CARTESIAN_POINT ( 'NONE',  ( 0.000000000000000000, 5.000000000000000000, 3.799999999999999822 ) ) ;
#14359 = EDGE_CURVE ( 'NONE', #8930, #4773, #10250, .T. ) ;
#14360 = ORIENTED_EDGE ( 'NONE', *, *, #10604, .F. ) ;
#14361 = ORIENTED_EDGE ( 'NONE', *, *, #5619, .F. ) ;
#14362 = DIRECTION ( 'NONE',  ( -1.000000000000000000, 0.000000000000000000, 0.000000000000000000 ) ) ;
#14363 = VECTOR ( 'NONE', #12951, 1000.000000000000000 ) ;
#14364 = CARTESIAN_POINT ( 'NONE',  ( 17.92752199202933738, 38.74634676501045760, 13.62426406871192874 ) ) ;
#14365 = ORIENTED_EDGE ( 'NONE', *, *, #6092, .F. ) ;
#14366 = AXIS2_PLACEMENT_3D ( 'NONE', #292, #8809, #3563 ) ;
#14367 = LINE ( 'NONE', #1054, #5652 ) ;
#14368 = EDGE_CURVE ( 'NONE', #2212, #16494, #16637, .T. ) ;
#14369 = ORIENTED_EDGE ( 'NONE', *, *, #15152, .F. ) ;
#14370 = DIRECTION ( 'NONE',  ( 0.000000000000000000, 1.000000000000000000, 0.000000000000000000 ) ) ;
#14371 = CARTESIAN_POINT ( 'NONE',  ( -1.774728116533986766, 43.31054587065082728, 37.66679706732590915 ) ) ;
#14372 = AXIS2_PLACEMENT_3D ( 'NONE', #559, #3952, #2358 ) ;
#14373 = FACE_OUTER_BOUND ( 'NONE', #1027, .T. ) ;
#14374 = DIRECTION ( 'NONE',  ( -0.000000000000000000, 1.000000000000000000, -0.000000000000000000 ) ) ;
#14375 = CARTESIAN_POINT ( 'NONE',  ( 3.627054932750481964, -33.43424481021354921, 68.00000000000000000 ) ) ;
#14376 = ORIENTED_EDGE ( 'NONE', *, *, #2668, .T. ) ;
#14377 = DIRECTION ( 'NONE',  ( -0.000000000000000000, -0.000000000000000000, -1.000000000000000000 ) ) ;
#14378 = LINE ( 'NONE', #21229, #14247 ) ;
#14379 = DIRECTION ( 'NONE',  ( 1.000000000000000000, 0.000000000000000000, -0.000000000000000000 ) ) ;
#14380 = CARTESIAN_POINT ( 'NONE',  ( 14.71174975910708049, 51.86873716947361856, 109.6002446535588319 ) ) ;
#14381 = ORIENTED_EDGE ( 'NONE', *, *, #9134, .F. ) ;
#14382 = SURFACE_STYLE_USAGE ( .BOTH. , #4545 ) ;
#14383 = EDGE_CURVE ( 'NONE', #15453, #3099, #12887, .T. ) ;
#14384 = ORIENTED_EDGE ( 'NONE', *, *, #8365, .T. ) ;
#14385 = DIRECTION ( 'NONE',  ( 0.000000000000000000, 0.000000000000000000, 1.000000000000000000 ) ) ;
#14386 = CARTESIAN_POINT ( 'NONE',  ( 34.39999999999998437, -85.00000000000000000, 0.3000000000000042077 ) ) ;
#14387 = ORIENTED_EDGE ( 'NONE', *, *, #6044, .T. ) ;
#14388 = ORIENTED_EDGE ( 'NONE', *, *, #224, .T. ) ;
#14389 = CARTESIAN_POINT ( 'NONE',  ( 1.824728116533979261, 43.31054587065082728, 39.70876104995653577 ) ) ;
#14390 = FACE_OUTER_BOUND ( 'NONE', #10878, .T. ) ;
#14391 = DIRECTION ( 'NONE',  ( -0.000000000000000000, -0.000000000000000000, -1.000000000000000000 ) ) ;
#14392 = ORIENTED_EDGE ( 'NONE', *, *, #19445, .T. ) ;
#14393 = ADVANCED_FACE ( 'NONE', ( #269 ), #10470, .T. ) ;
#14394 = EDGE_CURVE ( 'NONE', #4119, #2536, #5219, .T. ) ;
#14395 = ORIENTED_EDGE ( 'NONE', *, *, #6480, .T. ) ;
#14396 = DIRECTION ( 'NONE',  ( 0.000000000000000000, 1.000000000000000000, 0.000000000000000000 ) ) ;
#14397 = CARTESIAN_POINT ( 'NONE',  ( 1.724728116533979616, 43.26054587065083012, 27.70876104995653577 ) ) ;
#14398 = CARTESIAN_POINT ( 'NONE',  ( 1.774728116533979438, 43.31054587065082728, 35.80876104995653009 ) ) ;
#14399 = DIRECTION ( 'NONE',  ( 0.000000000000000000, 0.000000000000000000, 1.000000000000000000 ) ) ;
#14400 = DIRECTION ( 'NONE',  ( 0.000000000000000000, -1.000000000000000000, 0.000000000000000000 ) ) ;
#14401 = CARTESIAN_POINT ( 'NONE',  ( 1.724728116533979616, 43.26054587065083012, 29.76679706732590702 ) ) ;
#14402 = CARTESIAN_POINT ( 'NONE',  ( -29.37540678000427619, -6.000000000000000000, 3.799999999999999822 ) ) ;
#14403 = AXIS2_PLACEMENT_3D ( 'NONE', #8309, #15114, #21962 ) ;
#14404 = ORIENTED_EDGE ( 'NONE', *, *, #7526, .T. ) ;
#14405 = DIRECTION ( 'NONE',  ( 1.000000000000000000, 0.000000000000000000, 0.000000000000000000 ) ) ;
#14406 = ADVANCED_FACE ( 'NONE', ( #11908 ), #6914, .T. ) ;
#14407 = CARTESIAN_POINT ( 'NONE',  ( -9.718906393579157310, 43.49585613540820361, 70.88527860057354246 ) ) ;
#14408 = DIRECTION ( 'NONE',  ( 0.000000000000000000, 0.000000000000000000, 1.000000000000000000 ) ) ;
#14409 = DIRECTION ( 'NONE',  ( 0.000000000000000000, -1.000000000000000000, 0.000000000000000000 ) ) ;
#14410 = CARTESIAN_POINT ( 'NONE',  ( -18.22752199202934520, -39.04634676501046187, 13.50000000000000000 ) ) ;
#14411 = ORIENTED_EDGE ( 'NONE', *, *, #2648, .F. ) ;
#14412 = ORIENTED_EDGE ( 'NONE', *, *, #12873, .F. ) ;
#14413 = FACE_OUTER_BOUND ( 'NONE', #7521, .T. ) ;
#14414 = EDGE_CURVE ( 'NONE', #17175, #9565, #21857, .T. ) ;
#14415 = ORIENTED_EDGE ( 'NONE', *, *, #13017, .F. ) ;
#14416 = EDGE_CURVE ( 'NONE', #8846, #11165, #3268, .T. ) ;
#14417 = ORIENTED_EDGE ( 'NONE', *, *, #6398, .T. ) ;
#14418 = LINE ( 'NONE', #21934, #1677 ) ;
#14419 = ADVANCED_FACE ( 'NONE', ( #15488 ), #157, .T. ) ;
#14420 = DIRECTION ( 'NONE',  ( 1.224646799147353207E-16, 0.000000000000000000, 1.000000000000000000 ) ) ;
#14421 = ORIENTED_EDGE ( 'NONE', *, *, #7446, .T. ) ;
#14422 = DIRECTION ( 'NONE',  ( 0.000000000000000000, 0.000000000000000000, -1.000000000000000000 ) ) ;
#14423 = CARTESIAN_POINT ( 'NONE',  ( -15.21174975910705207, 51.61873716947361856, 68.00000000000000000 ) ) ;
#14424 = DIRECTION ( 'NONE',  ( 0.000000000000000000, -1.000000000000000000, 0.000000000000000000 ) ) ;
#14425 = PLANE ( 'NONE',  #7727 ) ;
#14426 = CARTESIAN_POINT ( 'NONE',  ( 29.37540678000427619, -6.000000000000000000, 3.500000000000000000 ) ) ;
#14427 = EDGE_CURVE ( 'NONE', #19370, #11890, #5609, .T. ) ;
#14428 = FACE_OUTER_BOUND ( 'NONE', #20714, .T. ) ;
#14429 = CARTESIAN_POINT ( 'NONE',  ( -1.774728116533986766, 42.36054587065083155, 27.70876104995653577 ) ) ;
#14430 = DIRECTION ( 'NONE',  ( 0.000000000000000000, 1.000000000000000000, 0.000000000000000000 ) ) ;
#14431 = FACE_BOUND ( 'NONE', #9199, .T. ) ;
#14432 = DIRECTION ( 'NONE',  ( 1.000000000000000000, 0.000000000000000000, 0.000000000000000000 ) ) ;
#14433 = CARTESIAN_POINT ( 'NONE',  ( -35.00000000000000000, -84.70000000000001705, 0.2999999999999999889 ) ) ;
#14434 = ORIENTED_EDGE ( 'NONE', *, *, #9863, .T. ) ;
#14435 = EDGE_LOOP ( 'NONE', ( #14522, #21106, #19176, #21765 ) ) ;
#14436 = FACE_OUTER_BOUND ( 'NONE', #21246, .T. ) ;
#14437 = ORIENTED_EDGE ( 'NONE', *, *, #6695, .T. ) ;
#14438 = EDGE_CURVE ( 'NONE', #11510, #7145, #12559, .T. ) ;
#14439 = ORIENTED_EDGE ( 'NONE', *, *, #20173, .F. ) ;
#14440 = EDGE_CURVE ( 'NONE', #8427, #8171, #5064, .T. ) ;
#14441 = AXIS2_PLACEMENT_3D ( 'NONE', #14723, #11246, #4549 ) ;
#14442 = AXIS2_PLACEMENT_3D ( 'NONE', #15886, #11192, #16215 ) ;
#14443 = CARTESIAN_POINT ( 'NONE',  ( -9.178906393579158163, 42.46645089659918426, 68.06527860057354928 ) ) ;
#14444 = CARTESIAN_POINT ( 'NONE',  ( 4.985331397971318523, 42.46645089659917716, 68.50000000000000000 ) ) ;
#14445 = ORIENTED_EDGE ( 'NONE', *, *, #17311, .T. ) ;
#14446 = CARTESIAN_POINT ( 'NONE',  ( -14.71174975910705029, 50.19799549595485644, 13.75000000000000000 ) ) ;
#14447 = CARTESIAN_POINT ( 'NONE',  ( 32.50000000000002132, 71.00000000000001421, 3.500000000000000000 ) ) ;
#14448 = CARTESIAN_POINT ( 'NONE',  ( -28.87540678000427619, 6.494748934539263274, 13.19999999999999929 ) ) ;
#14449 = CARTESIAN_POINT ( 'NONE',  ( -34.70000000000001705, -85.00000000000000000, 79.39999999999999147 ) ) ;
#14450 = CARTESIAN_POINT ( 'NONE',  ( 30.79999999999999716, -84.70000000000001705, 0.3000000000000039857 ) ) ;
#14451 = EDGE_CURVE ( 'NONE', #16854, #1657, #17206, .T. ) ;
#14452 = VERTEX_POINT ( 'NONE', #377 ) ;
#14453 = CARTESIAN_POINT ( 'NONE',  ( 28.87540678000427619, -6.494748934539263274, 13.19999999999999929 ) ) ;
#14454 = CARTESIAN_POINT ( 'NONE',  ( -20.53081511603577525, 86.49759185912193971, 68.50000000000000000 ) ) ;
#14455 = EDGE_CURVE ( 'NONE', #5434, #3729, #5547, .T. ) ;
#14456 = DIRECTION ( 'NONE',  ( 1.000000000000000000, 3.587913079599239526E-15, 0.000000000000000000 ) ) ;
#14457 = ORIENTED_EDGE ( 'NONE', *, *, #15691, .T. ) ;
#14458 = CIRCLE ( 'NONE', #16242, 0.5000000000000004441 ) ;
#14459 = ORIENTED_EDGE ( 'NONE', *, *, #11958, .F. ) ;
#14460 = AXIS2_PLACEMENT_3D ( 'NONE', #14818, #11364, #13024 ) ;
#14461 = ORIENTED_EDGE ( 'NONE', *, *, #15226, .T. ) ;
#14462 = DIRECTION ( 'NONE',  ( -1.000000000000000000, 0.000000000000000000, 0.000000000000000000 ) ) ;
#14463 = CARTESIAN_POINT ( 'NONE',  ( -28.57540678000427548, -63.74634676501045050, 13.19999999999999929 ) ) ;
#14464 = ORIENTED_EDGE ( 'NONE', *, *, #19169, .T. ) ;
#14465 = CARTESIAN_POINT ( 'NONE',  ( -17.95292532278785913, 50.11873716947361856, 13.99999999999999822 ) ) ;
#14466 = EDGE_LOOP ( 'NONE', ( #14086, #17061, #5527, #18352 ) ) ;
#14467 = AXIS2_PLACEMENT_3D ( 'NONE', #4693, #764, #14635 ) ;
#14468 = CARTESIAN_POINT ( 'NONE',  ( 0.000000000000000000, -84.70000000000001705, 78.79999999999999716 ) ) ;
#14469 = CARTESIAN_POINT ( 'NONE',  ( -25.37540678000427263, 63.74634676501045050, 7.200000000000000178 ) ) ;
#14470 = DIRECTION ( 'NONE',  ( 0.000000000000000000, 0.000000000000000000, -1.000000000000000000 ) ) ;
#14471 = AXIS2_PLACEMENT_3D ( 'NONE', #15158, #11800, #5548 ) ;
#14472 = LINE ( 'NONE', #943, #1835 ) ;
#14473 = VECTOR ( 'NONE', #16481, 1000.000000000000000 ) ;
#14474 = CARTESIAN_POINT ( 'NONE',  ( 0.000000000000000000, 32.11873716947361856, 109.6002446535588319 ) ) ;
#14475 = AXIS2_PLACEMENT_3D ( 'NONE', #4210, #9351, #7250 ) ;
#14476 = ORIENTED_EDGE ( 'NONE', *, *, #20274, .F. ) ;
#14477 = CARTESIAN_POINT ( 'NONE',  ( -29.37540678000427619, -6.000000000000000000, 3.799999999999999822 ) ) ;
#14478 = LINE ( 'NONE', #12917, #14598 ) ;
#14479 = CARTESIAN_POINT ( 'NONE',  ( -8.638906393579159015, 40.01645089659919563, 70.88527860057354246 ) ) ;
#14480 = CARTESIAN_POINT ( 'NONE',  ( -23.26721486835118569, -3.307416615798745685, 13.50000000000000355 ) ) ;
#14481 = ORIENTED_EDGE ( 'NONE', *, *, #7174, .F. ) ;
#14482 = DIRECTION ( 'NONE',  ( -1.000000000000000000, 0.000000000000000000, 0.000000000000000000 ) ) ;
#14483 = ORIENTED_EDGE ( 'NONE', *, *, #9475, .F. ) ;
#14484 = PLANE ( 'NONE',  #14441 ) ;
#14485 = FACE_OUTER_BOUND ( 'NONE', #7818, .T. ) ;
#14486 = EDGE_CURVE ( 'NONE', #4912, #3263, #15705, .T. ) ;
#14487 = ORIENTED_EDGE ( 'NONE', *, *, #14328, .F. ) ;
#14488 = TOROIDAL_SURFACE ( 'NONE', #3446, 0.05000000000000000278, 0.05000000000000000278 ) ;
#14489 = VECTOR ( 'NONE', #3119, 1000.000000000000000 ) ;
#14490 = AXIS2_PLACEMENT_3D ( 'NONE', #3496, #10332, #5952 ) ;
#14491 = VERTEX_POINT ( 'NONE', #10893 ) ;
#14492 = CARTESIAN_POINT ( 'NONE',  ( -29.13662752439705272, -5.299999999999999822, 7.200000000000000178 ) ) ;
#14493 = CARTESIAN_POINT ( 'NONE',  ( 15.95292532278785913, -51.61873716947361856, 14.00000000000000000 ) ) ;
#14494 = DIRECTION ( 'NONE',  ( -1.000000000000000000, -0.000000000000000000, -0.000000000000000000 ) ) ;
#14495 = AXIS2_PLACEMENT_3D ( 'NONE', #6181, #6071, #13077 ) ;
#14496 = ORIENTED_EDGE ( 'NONE', *, *, #2404, .T. ) ;
#14497 = AXIS2_PLACEMENT_3D ( 'NONE', #13013, #11132, #2630 ) ;
#14498 = EDGE_LOOP ( 'NONE', ( #11892, #1924, #12803, #12896 ) ) ;
#14499 = DIRECTION ( 'NONE',  ( 0.000000000000000000, -1.000000000000000000, 0.000000000000000000 ) ) ;
#14500 = ORIENTED_EDGE ( 'NONE', *, *, #21645, .F. ) ;
#14501 = FACE_OUTER_BOUND ( 'NONE', #18836, .T. ) ;
#14502 = EDGE_CURVE ( 'NONE', #14785, #10729, #3978, .T. ) ;
#14503 = AXIS2_PLACEMENT_3D ( 'NONE', #2971, #16721, #1066 ) ;
#14504 = AXIS2_PLACEMENT_3D ( 'NONE', #9809, #22134, #13605 ) ;
#14505 = DIRECTION ( 'NONE',  ( 1.000000000000000000, 0.000000000000000000, 0.000000000000000000 ) ) ;
#14506 = AXIS2_PLACEMENT_3D ( 'NONE', #1117, #4047, #2355 ) ;
#14507 = CARTESIAN_POINT ( 'NONE',  ( 29.09616841400578124, 6.500357067309672665, 7.499999999999999112 ) ) ;
#14508 = FACE_OUTER_BOUND ( 'NONE', #15513, .T. ) ;
#14509 = DIRECTION ( 'NONE',  ( 0.000000000000000000, 0.000000000000000000, 1.000000000000000000 ) ) ;
#14510 = ORIENTED_EDGE ( 'NONE', *, *, #2250, .T. ) ;
#14511 = LINE ( 'NONE', #19913, #10206 ) ;
#14512 = AXIS2_PLACEMENT_3D ( 'NONE', #7974, #2931, #14335 ) ;
#14513 = EDGE_CURVE ( 'NONE', #21455, #8790, #21209, .T. ) ;
#14514 = CARTESIAN_POINT ( 'NONE',  ( 0.000000000000000000, 42.31054587065082728, 37.71679706732590631 ) ) ;
#14515 = CYLINDRICAL_SURFACE ( 'NONE', #13302, 0.2999999999999947153 ) ;
#14516 = DIRECTION ( 'NONE',  ( -1.000000000000000000, 0.000000000000000000, 0.000000000000000000 ) ) ;
#14517 = CARTESIAN_POINT ( 'NONE',  ( -32.23382792203229741, 83.71979900898287497, 13.75000000000000000 ) ) ;
#14518 = VERTEX_POINT ( 'NONE', #10690 ) ;
#14519 = VECTOR ( 'NONE', #4981, 1000.000000000000000 ) ;
#14520 = AXIS2_PLACEMENT_3D ( 'NONE', #20584, #18907, #3578 ) ;
#14521 = CIRCLE ( 'NONE', #18463, 0.5000000000000004441 ) ;
#14522 = ORIENTED_EDGE ( 'NONE', *, *, #13703, .T. ) ;
#14523 = DIRECTION ( 'NONE',  ( 0.000000000000000000, 0.000000000000000000, 1.000000000000000000 ) ) ;
#14524 = CONTEXT_DEPENDENT_SHAPE_REPRESENTATION ( #1560, #3599 ) ;
#14525 = EDGE_LOOP ( 'NONE', ( #11480, #19795, #16383, #17528 ) ) ;
#14526 = ORIENTED_EDGE ( 'NONE', *, *, #10081, .F. ) ;
#14527 = AXIS2_PLACEMENT_3D ( 'NONE', #11915, #3321, #17076 ) ;
#14528 = EDGE_CURVE ( 'NONE', #4392, #11429, #12172, .T. ) ;
#14529 = PLANE ( 'NONE',  #6530 ) ;
#14530 = EDGE_LOOP ( 'NONE', ( #8530, #8587, #12014, #8076 ) ) ;
#14531 = DIRECTION ( 'NONE',  ( -0.9510565162951554186, 0.000000000000000000, 0.3090169943749416781 ) ) ;
#14532 = ORIENTED_EDGE ( 'NONE', *, *, #15959, .T. ) ;
#14533 = CARTESIAN_POINT ( 'NONE',  ( -4.985331397971318523, 42.46645089659917716, 69.50000000000000000 ) ) ;
#14534 = CARTESIAN_POINT ( 'NONE',  ( 28.57540678000427548, 63.74634676501045050, 13.50000000000000000 ) ) ;
#14535 = LINE ( 'NONE', #9518, #20233 ) ;
#14536 = AXIS2_PLACEMENT_3D ( 'NONE', #13441, #20282, #8867 ) ;
#14537 = CIRCLE ( 'NONE', #20278, 0.2500000000000002220 ) ;
#14538 = AXIS2_PLACEMENT_3D ( 'NONE', #11280, #21496, #9839 ) ;
#14539 = DIRECTION ( 'NONE',  ( 1.000000000000000000, 0.000000000000000000, 0.000000000000000000 ) ) ;
#14540 = EDGE_CURVE ( 'NONE', #471, #3217, #9330, .T. ) ;
#14541 = EDGE_CURVE ( 'NONE', #14287, #12166, #5990, .T. ) ;
#14542 = DIRECTION ( 'NONE',  ( -0.000000000000000000, -0.000000000000000000, 1.000000000000000000 ) ) ;
#14543 = EDGE_CURVE ( 'NONE', #15631, #5063, #11830, .T. ) ;
#14544 = FACE_OUTER_BOUND ( 'NONE', #10069, .T. ) ;
#14545 = CARTESIAN_POINT ( 'NONE',  ( -1.724728116533986721, 42.31054587065082728, 31.75876104995653648 ) ) ;
#14546 = DIRECTION ( 'NONE',  ( -0.000000000000000000, -1.000000000000000000, -0.000000000000000000 ) ) ;
#14547 = AXIS2_PLACEMENT_3D ( 'NONE', #9114, #12458, #19085 ) ;
#14548 = EDGE_CURVE ( 'NONE', #22083, #16682, #20779, .T. ) ;
#14549 = VECTOR ( 'NONE', #15495, 1000.000000000000000 ) ;
#14550 = ORIENTED_EDGE ( 'NONE', *, *, #16950, .F. ) ;
#14551 = CYLINDRICAL_SURFACE ( 'NONE', #2737, 5.000000000000000888 ) ;
#14552 = DIRECTION ( 'NONE',  ( 0.000000000000000000, 0.000000000000000000, -1.000000000000000000 ) ) ;
#14553 = ORIENTED_EDGE ( 'NONE', *, *, #1756, .F. ) ;
#14554 = ORIENTED_EDGE ( 'NONE', *, *, #8035, .T. ) ;
#14555 = DIRECTION ( 'NONE',  ( 0.000000000000000000, 1.000000000000000000, 0.000000000000000000 ) ) ;
#14556 = CARTESIAN_POINT ( 'NONE',  ( 15.95292532278785913, -32.11873716947361856, 68.50000000000000000 ) ) ;
#14557 = EDGE_LOOP ( 'NONE', ( #16759, #727, #1286, #4044 ) ) ;
#14558 = AXIS2_PLACEMENT_3D ( 'NONE', #20223, #11711, #14839 ) ;
#14559 = AXIS2_PLACEMENT_3D ( 'NONE', #7160, #12599, #189 ) ;
#14560 = CARTESIAN_POINT ( 'NONE',  ( -19.16037735075775217, 42.46645089659918426, 13.50000000000000000 ) ) ;
#14561 = ORIENTED_EDGE ( 'NONE', *, *, #2991, .T. ) ;
#14562 = ADVANCED_FACE ( 'NONE', ( #7332 ), #1467, .F. ) ;
#14563 = AXIS2_PLACEMENT_3D ( 'NONE', #20488, #14996, #4810 ) ;
#14564 = CIRCLE ( 'NONE', #10653, 0.05000000000000143219 ) ;
#14565 = VECTOR ( 'NONE', #10486, 1000.000000000000000 ) ;
#14566 = APPLICATION_CONTEXT ( 'automotive_design' ) ;
#14567 = CARTESIAN_POINT ( 'NONE',  ( -17.93704824106378837, -38.74634676501045760, 13.87500000000000000 ) ) ;
#14568 = DIRECTION ( 'NONE',  ( -0.000000000000000000, -0.000000000000000000, -1.000000000000000000 ) ) ;
#14569 = ORIENTED_EDGE ( 'NONE', *, *, #20047, .F. ) ;
#14570 = CARTESIAN_POINT ( 'NONE',  ( 18.22752199202934520, -39.04634676501046187, 13.50000000000000000 ) ) ;
#14571 = DIRECTION ( 'NONE',  ( 1.000000000000000000, 0.000000000000000000, 0.000000000000000000 ) ) ;
#14572 = EDGE_CURVE ( 'NONE', #7627, #258, #13629, .T. ) ;
#14573 = CARTESIAN_POINT ( 'NONE',  ( -17.45292532278785913, 50.11873716947361856, 14.00000000000000000 ) ) ;
#14574 = DIRECTION ( 'NONE',  ( 0.000000000000000000, 0.000000000000000000, 1.000000000000000000 ) ) ;
#14575 = VECTOR ( 'NONE', #19647, 1000.000000000000000 ) ;
#14576 = CARTESIAN_POINT ( 'NONE',  ( -23.02398829872514341, 3.262290859344318950, 13.79999999999999893 ) ) ;
#14577 = ADVANCED_FACE ( 'NONE', ( #19405 ), #17712, .T. ) ;
#14578 = EDGE_LOOP ( 'NONE', ( #8334, #21558, #17014, #16316, #459, #9230, #15375, #17504, #9148, #10249, #16196, #10983, #15443, #15129, #20576, #5836, #7719, #6166, #11835, #3334, #10828, #3875, #19260, #9260, #1617, #19306, #12558, #16648, #3044, #18486, #21848, #18366, #12077, #883, #18427, #2067, #15771, #19987, #7524, #1244, #3933, #1995, #4753, #11007, #20808, #1984, #14101, #14717, #11545, #1613, #2578, #2735, #3374, #6890, #13660, #10403, #19339, #17337, #19100, #19244, #21057, #102, #1880, #18399 ) ) ;
#14579 = DIRECTION ( 'NONE',  ( -1.000000000000000000, 0.000000000000000000, 0.000000000000000000 ) ) ;
#14580 = DIRECTION ( 'NONE',  ( -2.107255972849994642E-16, 0.000000000000000000, -1.000000000000000000 ) ) ;
#14581 = VECTOR ( 'NONE', #16864, 1000.000000000000000 ) ;
#14582 = ORIENTED_EDGE ( 'NONE', *, *, #6505, .T. ) ;
#14583 = ORIENTED_EDGE ( 'NONE', *, *, #3254, .F. ) ;
#14584 = AXIS2_PLACEMENT_3D ( 'NONE', #5839, #2463, #21268 ) ;
#14585 = EDGE_LOOP ( 'NONE', ( #4342, #1957, #6476, #17656 ) ) ;
#14586 = FACE_OUTER_BOUND ( 'NONE', #20329, .T. ) ;
#14587 = CIRCLE ( 'NONE', #20325, 0.04999999999999991257 ) ;
#14588 = CARTESIAN_POINT ( 'NONE',  ( 17.92752199202934094, 38.74634676501045760, 13.79999999999999893 ) ) ;
#14589 = ORIENTED_EDGE ( 'NONE', *, *, #9818, .T. ) ;
#14590 = FACE_OUTER_BOUND ( 'NONE', #3368, .T. ) ;
#14591 = ORIENTED_EDGE ( 'NONE', *, *, #2365, .T. ) ;
#14592 = DIRECTION ( 'NONE',  ( -0.000000000000000000, 0.000000000000000000, 1.000000000000000000 ) ) ;
#14593 = VECTOR ( 'NONE', #15182, 1000.000000000000000 ) ;
#14594 = DIRECTION ( 'NONE',  ( 0.000000000000000000, 0.000000000000000000, -1.000000000000000000 ) ) ;
#14595 = EDGE_CURVE ( 'NONE', #8145, #7855, #16029, .T. ) ;
#14596 = DIRECTION ( 'NONE',  ( -1.000000000000000000, 0.000000000000000000, 0.000000000000000000 ) ) ;
#14597 = LINE ( 'NONE', #21451, #6297 ) ;
#14598 = VECTOR ( 'NONE', #19764, 1000.000000000000000 ) ;
#14599 = CARTESIAN_POINT ( 'NONE',  ( -30.37540678000427619, -6.000000000000000000, 3.799999999999999822 ) ) ;
#14600 = DIRECTION ( 'NONE',  ( 0.000000000000000000, 0.000000000000000000, -1.000000000000000000 ) ) ;
#14601 = ORIENTED_EDGE ( 'NONE', *, *, #11473, .F. ) ;
#14602 = CYLINDRICAL_SURFACE ( 'NONE', #10600, 0.5000000000000004441 ) ;
#14603 = CIRCLE ( 'NONE', #977, 1.974596669241483804 ) ;
#14604 = DIRECTION ( 'NONE',  ( 0.000000000000000000, 0.000000000000000000, -1.000000000000000000 ) ) ;
#14605 = CARTESIAN_POINT ( 'NONE',  ( -1.724728116533986721, 42.31054587065082728, 41.71679706732590631 ) ) ;
#14606 = LINE ( 'NONE', #1069, #17947 ) ;
#14607 = EDGE_LOOP ( 'NONE', ( #22022, #2441, #15193, #6686 ) ) ;
#14608 = CARTESIAN_POINT ( 'NONE',  ( 15.95292532278785913, -32.61873716947361856, 68.50000000000000000 ) ) ;
#14609 = DIRECTION ( 'NONE',  ( 0.000000000000000000, 0.000000000000000000, -1.000000000000000000 ) ) ;
#14610 = EDGE_CURVE ( 'NONE', #8484, #13135, #21763, .T. ) ;
#14611 = ORIENTED_EDGE ( 'NONE', *, *, #10171, .F. ) ;
#14612 = DIRECTION ( 'NONE',  ( -1.000000000000000000, 0.000000000000000000, -0.000000000000000000 ) ) ;
#14613 = CARTESIAN_POINT ( 'NONE',  ( -34.40000000000001279, -85.00000000000000000, 79.70000000000000284 ) ) ;
#14614 = ORIENTED_EDGE ( 'NONE', *, *, #7176, .F. ) ;
#14615 = EDGE_LOOP ( 'NONE', ( #2575, #2561, #16139, #16912 ) ) ;
#14616 = CARTESIAN_POINT ( 'NONE',  ( -1.836970198721042383E-17, 84.70000000000001705, 0.3000000000000021538 ) ) ;
#14617 = DIRECTION ( 'NONE',  ( 0.000000000000000000, -1.000000000000000000, 0.000000000000000000 ) ) ;
#14618 = FACE_OUTER_BOUND ( 'NONE', #20214, .T. ) ;
#14619 = VECTOR ( 'NONE', #18574, 1000.000000000000000 ) ;
#14620 = ORIENTED_EDGE ( 'NONE', *, *, #8966, .F. ) ;
#14621 = ORIENTED_EDGE ( 'NONE', *, *, #13614, .T. ) ;
#14622 = CARTESIAN_POINT ( 'NONE',  ( -31.44597781366222122, 58.94165929845684815, 68.75000000000000000 ) ) ;
#14623 = EDGE_CURVE ( 'NONE', #8916, #7522, #6144, .T. ) ;
#14624 = DIRECTION ( 'NONE',  ( 0.000000000000000000, 0.000000000000000000, -1.000000000000000000 ) ) ;
#14625 = CARTESIAN_POINT ( 'NONE',  ( -23.04273166366764514, -2.261511273150494716, 13.23427437508502358 ) ) ;
#14626 = ADVANCED_FACE ( 'NONE', ( #1373 ), #13120, .T. ) ;
#14627 = VECTOR ( 'NONE', #8780, 1000.000000000000000 ) ;
#14628 = FACE_OUTER_BOUND ( 'NONE', #516, .T. ) ;
#14629 = PLANE ( 'NONE',  #21536 ) ;
#14630 = CARTESIAN_POINT ( 'NONE',  ( -14.66174975910705136, 51.76873716947361714, 13.50000000000000000 ) ) ;
#14631 = AXIS2_PLACEMENT_3D ( 'NONE', #15559, #14001, #15680 ) ;
#14632 = AXIS2_PLACEMENT_3D ( 'NONE', #17618, #9020, #20776 ) ;
#14633 = DIRECTION ( 'NONE',  ( -0.000000000000000000, -0.000000000000000000, -1.000000000000000000 ) ) ;
#14634 = ORIENTED_EDGE ( 'NONE', *, *, #13185, .F. ) ;
#14635 = DIRECTION ( 'NONE',  ( 1.000000000000000000, 0.000000000000000000, 0.000000000000000000 ) ) ;
#14636 = CARTESIAN_POINT ( 'NONE',  ( 1.724728116533979838, 42.36054587065083155, 45.66679706732590205 ) ) ;
#14637 = FACE_OUTER_BOUND ( 'NONE', #4776, .T. ) ;
#14638 = CARTESIAN_POINT ( 'NONE',  ( -29.13662752439705272, 0.000000000000000000, 3.799999999999999822 ) ) ;
#14639 = DIRECTION ( 'NONE',  ( -8.673617379884034239E-17, -0.000000000000000000, 1.000000000000000000 ) ) ;
#14640 = ORIENTED_EDGE ( 'NONE', *, *, #14275, .F. ) ;
#14641 = EDGE_CURVE ( 'NONE', #799, #15862, #14336, .T. ) ;
#14642 = EDGE_LOOP ( 'NONE', ( #19574, #8763, #19093, #4829 ) ) ;
#14643 = LINE ( 'NONE', #6276, #12437 ) ;
#14644 = TOROIDAL_SURFACE ( 'NONE', #10734, 4.700000000000004619, 0.2999999999999999889 ) ;
#14645 = VECTOR ( 'NONE', #10386, 1000.000000000000000 ) ;
#14646 = CIRCLE ( 'NONE', #10393, 2.500000000000002220 ) ;
#14647 = ORIENTED_EDGE ( 'NONE', *, *, #6545, .T. ) ;
#14648 = ADVANCED_FACE ( 'NONE', ( #14691 ), #5789, .T. ) ;
#14649 = FACE_OUTER_BOUND ( 'NONE', #872, .T. ) ;
#14650 = ORIENTED_EDGE ( 'NONE', *, *, #21017, .T. ) ;
#14651 = DIRECTION ( 'NONE',  ( 1.000000000000000000, 0.000000000000000000, 0.000000000000000000 ) ) ;
#14652 = CARTESIAN_POINT ( 'NONE',  ( 8.641460742840918030, 32.93424481021354921, 68.00000000000000000 ) ) ;
#14653 = LINE ( 'NONE', #21511, #17358 ) ;
#14654 = CARTESIAN_POINT ( 'NONE',  ( -1.774728116533986766, 42.31054587065082728, 53.66679706732590915 ) ) ;
#14655 = CARTESIAN_POINT ( 'NONE',  ( -14.66174975910705136, 0.000000000000000000, 13.50000000000000000 ) ) ;
#14656 = DIRECTION ( 'NONE',  ( 1.000000000000000000, -0.000000000000000000, -0.000000000000000000 ) ) ;
#14657 = TOROIDAL_SURFACE ( 'NONE', #5038, 2.299999999999993161, 0.2999999999999999889 ) ;
#14658 = CIRCLE ( 'NONE', #10407, 0.2500000000000002220 ) ;
#14659 = DIRECTION ( 'NONE',  ( 0.000000000000000000, -0.000000000000000000, -1.000000000000000000 ) ) ;
#14660 = FACE_OUTER_BOUND ( 'NONE', #368, .T. ) ;
#14661 = DIRECTION ( 'NONE',  ( 0.000000000000000000, 0.000000000000000000, -1.000000000000000000 ) ) ;
#14662 = EDGE_CURVE ( 'NONE', #3680, #12999, #52, .T. ) ;
#14663 = ORIENTED_EDGE ( 'NONE', *, *, #748, .T. ) ;
#14664 = CARTESIAN_POINT ( 'NONE',  ( -25.37540678000427263, -63.74634676501045050, 13.50000000000000000 ) ) ;
#14665 = CARTESIAN_POINT ( 'NONE',  ( -17.45292532278785913, 39.04634676501046187, 13.50000000000000000 ) ) ;
#14666 = EDGE_LOOP ( 'NONE', ( #4369, #6443, #5138, #19745 ) ) ;
#14667 = VERTEX_POINT ( 'NONE', #6554 ) ;
#14668 = CARTESIAN_POINT ( 'NONE',  ( 31.50000000000002132, -71.70000000000001705, 3.200000000000000178 ) ) ;
#14669 = DIRECTION ( 'NONE',  ( 0.000000000000000000, 0.000000000000000000, 1.000000000000000000 ) ) ;
#14670 = ORIENTED_EDGE ( 'NONE', *, *, #11746, .T. ) ;
#14671 = VERTEX_POINT ( 'NONE', #6211 ) ;
#14672 = CARTESIAN_POINT ( 'NONE',  ( -3.627054932750481964, 33.43424481021354921, 42.50000000000000000 ) ) ;
#14673 = ORIENTED_EDGE ( 'NONE', *, *, #8738, .T. ) ;
#14674 = EDGE_CURVE ( 'NONE', #11560, #4673, #11657, .T. ) ;
#14675 = EDGE_CURVE ( 'NONE', #18906, #1545, #7570, .T. ) ;
#14676 = AXIS2_PLACEMENT_3D ( 'NONE', #79, #5353, #13381 ) ;
#14677 = EDGE_CURVE ( 'NONE', #5889, #16679, #6321, .T. ) ;
#14678 = EDGE_LOOP ( 'NONE', ( #7, #15301, #4014, #10146 ) ) ;
#14679 = CARTESIAN_POINT ( 'NONE',  ( 15.16923466928735742, -52.00603548408893317, 13.50000000000000000 ) ) ;
#14680 = DIRECTION ( 'NONE',  ( 0.000000000000000000, 0.000000000000000000, 1.000000000000000000 ) ) ;
#14681 = ORIENTED_EDGE ( 'NONE', *, *, #18303, .F. ) ;
#14682 = FILL_AREA_STYLE_COLOUR ( '', #3951 ) ;
#14683 = AXIS2_PLACEMENT_3D ( 'NONE', #5210, #17171, #58 ) ;
#14684 = DIRECTION ( 'NONE',  ( 1.000000000000000000, 3.052134192567374827E-16, 0.000000000000000000 ) ) ;
#14685 = VECTOR ( 'NONE', #12128, 1000.000000000000000 ) ;
#14686 = CARTESIAN_POINT ( 'NONE',  ( -1.774728116533986766, 43.31054587065082728, 49.66679706732590915 ) ) ;
#14687 =( BOUNDED_SURFACE ( )  B_SPLINE_SURFACE ( 3, 2, ( 
 ( #11159, #2655, #21810 ),
 ( #971, #14739, #14625 ),
 ( #13174, #12939, #4682 ),
 ( #9722, #11386, #19787 ),
 ( #4447, #21590, #4566 ),
 ( #14961, #2995, #18212 ),
 ( #16524, #2895, #16625 ),
 ( #1300, #6487, #4787 ),
 ( #3558, #5238, #12032 ),
 ( #22149, #4897, #18883 ),
 ( #20224, #22023, #8805 ),
 ( #11712, #1762, #11926 ) ),
 .UNSPECIFIED., .F., .F., .F. ) 
 B_SPLINE_SURFACE_WITH_KNOTS ( ( 4, 2, 2, 2, 2, 4 ),
 ( 3, 3 ),
 ( 0.0007953085288493463639, 0.0009951922240469452709, 0.001195075919244544069, 0.001594843309639741667, 0.001994610700034939264, 0.002394378090430136861 ),
 ( 0.000000000000000000, 1.000000000000000000 ),
 .UNSPECIFIED. ) 
 GEOMETRIC_REPRESENTATION_ITEM ( )  RATIONAL_B_SPLINE_SURFACE ( (
 ( 1.000000000000000000, 0.9842566880020464648, 1.000000000000000000),
 ( 1.000000000000000000, 0.9842682545141110406, 1.000000000000000000),
 ( 1.000000000000000000, 0.9790935905989442967, 1.000000000000000000),
 ( 1.000000000000000000, 0.9652215946044103712, 1.000000000000000000),
 ( 1.000000000000000000, 0.9566241109334496784, 1.000000000000000000),
 ( 1.000000000000000000, 0.9283687200450407850, 1.000000000000000000),
 ( 1.000000000000000000, 0.9065874062052604598, 1.000000000000000000),
 ( 1.000000000000000000, 0.8577429740253560420, 1.000000000000000000),
 ( 1.000000000000000000, 0.8312249658972131749, 1.000000000000000000),
 ( 1.000000000000000000, 0.7732701221514807211, 1.000000000000000000),
 ( 1.000000000000000000, 0.7418345472257018569, 1.000000000000000000),
 ( 1.000000000000000000, 0.7071067811865475727, 1.000000000000000000) ) ) 
 REPRESENTATION_ITEM ( '' )  SURFACE ( )  );
#14688 = CARTESIAN_POINT ( 'NONE',  ( -1.724728116533986721, 42.31054587065082728, 37.71679706732590631 ) ) ;
#14689 = EDGE_CURVE ( 'NONE', #8961, #12734, #3658, .T. ) ;
#14690 = EDGE_LOOP ( 'NONE', ( #484, #13555, #20394 ) ) ;
#14691 = FACE_OUTER_BOUND ( 'NONE', #1870, .T. ) ;
#14692 = CARTESIAN_POINT ( 'NONE',  ( -30.37540678000427619, 0.000000000000000000, 7.200000000000000178 ) ) ;
#14693 = ORIENTED_EDGE ( 'NONE', *, *, #7886, .T. ) ;
#14694 = ORIENTED_EDGE ( 'NONE', *, *, #13925, .F. ) ;
#14695 = ORIENTED_EDGE ( 'NONE', *, *, #2311, .T. ) ;
#14696 = CARTESIAN_POINT ( 'NONE',  ( 0.000000000000000000, 42.31054587065082728, 39.75876104995654003 ) ) ;
#14697 = CARTESIAN_POINT ( 'NONE',  ( 31.50000000000002132, 72.00000000000001421, 3.200000000000000178 ) ) ;
#14698 = ORIENTED_EDGE ( 'NONE', *, *, #15888, .T. ) ;
#14699 = AXIS2_PLACEMENT_3D ( 'NONE', #12121, #18973, #261 ) ;
#14700 = DIRECTION ( 'NONE',  ( -1.000000000000000000, 0.000000000000000000, 0.000000000000000000 ) ) ;
#14701 = EDGE_CURVE ( 'NONE', #11864, #21336, #4638, .T. ) ;
#14702 = AXIS2_PLACEMENT_3D ( 'NONE', #8897, #17821, #15701 ) ;
#14703 = CIRCLE ( 'NONE', #13641, 4.699999999999999289 ) ;
#14704 = EDGE_CURVE ( 'NONE', #13975, #4058, #923, .T. ) ;
#14705 = ORIENTED_EDGE ( 'NONE', *, *, #11112, .T. ) ;
#14706 = DIRECTION ( 'NONE',  ( 1.000000000000000000, 0.000000000000000000, 0.000000000000000000 ) ) ;
#14707 = DIRECTION ( 'NONE',  ( 0.000000000000000000, 0.000000000000000000, 1.000000000000000000 ) ) ;
#14708 = EDGE_CURVE ( 'NONE', #7686, #1621, #13341, .T. ) ;
#14709 = DIRECTION ( 'NONE',  ( 1.000000000000000000, 0.000000000000000000, 0.000000000000000000 ) ) ;
#14710 = DIRECTION ( 'NONE',  ( 0.000000000000000000, 0.000000000000000000, 1.000000000000000000 ) ) ;
#14711 = DIRECTION ( 'NONE',  ( 1.301042606982568087E-14, 0.000000000000000000, 1.000000000000000000 ) ) ;
#14712 = ORIENTED_EDGE ( 'NONE', *, *, #21195, .T. ) ;
#14713 = CARTESIAN_POINT ( 'NONE',  ( 15.95292532278785913, -34.11873716947361856, 68.00000000000000000 ) ) ;
#14714 = CARTESIAN_POINT ( 'NONE',  ( 26.61833302554978786, -9.663695060508651125, 13.79999999999999893 ) ) ;
#14715 = FACE_OUTER_BOUND ( 'NONE', #3794, .T. ) ;
#14716 = LINE ( 'NONE', #2873, #20827 ) ;
#14717 = ORIENTED_EDGE ( 'NONE', *, *, #1509, .T. ) ;
#14718 = CARTESIAN_POINT ( 'NONE',  ( -15.21174975910705207, -52.11873716947361856, 14.00000000000000000 ) ) ;
#14719 = CARTESIAN_POINT ( 'NONE',  ( 33.49999999999999289, -84.70000000000001705, 1.799999999999996048 ) ) ;
#14720 = AXIS2_PLACEMENT_3D ( 'NONE', #21846, #6521, #5160 ) ;
#14721 = ADVANCED_FACE ( 'NONE', ( #21545 ), #18642, .T. ) ;
#14722 = ORIENTED_EDGE ( 'NONE', *, *, #17306, .F. ) ;
#14723 = CARTESIAN_POINT ( 'NONE',  ( 1.824728116533979261, 43.31054587065082728, 35.70876104995653577 ) ) ;
#14724 = CIRCLE ( 'NONE', #13655, 0.6000000000000033085 ) ;
#14725 = EDGE_CURVE ( 'NONE', #20218, #11552, #4512, .T. ) ;
#14726 = EDGE_LOOP ( 'NONE', ( #10901, #9683, #12091, #11481 ) ) ;
#14727 = ORIENTED_EDGE ( 'NONE', *, *, #13100, .F. ) ;
#14728 = ORIENTED_EDGE ( 'NONE', *, *, #2142, .T. ) ;
#14729 = CARTESIAN_POINT ( 'NONE',  ( -15.95292532278785913, 52.11873716947361856, 13.99999999999999822 ) ) ;
#14730 = CARTESIAN_POINT ( 'NONE',  ( -1.724728116533986721, 43.31054587065082728, 37.71679706732590631 ) ) ;
#14731 = EDGE_CURVE ( 'NONE', #12166, #1070, #6514, .T. ) ;
#14732 = DIRECTION ( 'NONE',  ( -2.107255972849994642E-16, 0.000000000000000000, -1.000000000000000000 ) ) ;
#14733 = ORIENTED_EDGE ( 'NONE', *, *, #10731, .T. ) ;
#14734 = ORIENTED_EDGE ( 'NONE', *, *, #8769, .T. ) ;
#14735 = DIRECTION ( 'NONE',  ( 0.000000000000000000, 1.000000000000000000, 0.000000000000000000 ) ) ;
#14736 = EDGE_CURVE ( 'NONE', #15983, #4059, #9000, .T. ) ;
#14737 = AXIS2_PLACEMENT_3D ( 'NONE', #8843, #17326, #14080 ) ;
#14738 = CARTESIAN_POINT ( 'NONE',  ( -1.824728116533986810, 43.31054587065082728, 45.76679706732590347 ) ) ;
#14739 = CARTESIAN_POINT ( 'NONE',  ( -23.02398829872489827, -2.211005466174399636, 13.25091654438544531 ) ) ;
#14740 = CIRCLE ( 'NONE', #9381, 0.2999999999999999334 ) ;
#14741 = DIRECTION ( 'NONE',  ( 1.000000000000000000, 0.000000000000000000, -0.000000000000000000 ) ) ;
#14742 = LINE ( 'NONE', #9725, #16773 ) ;
#14743 = LINE ( 'NONE', #12943, #12927 ) ;
#14744 = VERTEX_POINT ( 'NONE', #18277 ) ;
#14745 = DIRECTION ( 'NONE',  ( -1.000000000000000000, 1.094601647044990554E-16, -0.000000000000000000 ) ) ;
#14746 = CARTESIAN_POINT ( 'NONE',  ( 9.641460742840918030, 32.11873716947361856, 68.50000000000000000 ) ) ;
#14747 = CARTESIAN_POINT ( 'NONE',  ( -8.641460742840918030, 33.43424481021354921, 42.50000000000000000 ) ) ;
#14748 = ORIENTED_EDGE ( 'NONE', *, *, #345, .T. ) ;
#14749 = DIRECTION ( 'NONE',  ( -1.000000000000000000, 0.000000000000000000, 0.000000000000000000 ) ) ;
#14750 = CARTESIAN_POINT ( 'NONE',  ( -3.127054932750481964, 32.11873716947361856, 68.50000000000000000 ) ) ;
#14751 = CYLINDRICAL_SURFACE ( 'NONE', #20481, 0.04999999999999991257 ) ;
#14752 = ORIENTED_EDGE ( 'NONE', *, *, #19222, .T. ) ;
#14753 = CYLINDRICAL_SURFACE ( 'NONE', #12439, 0.2500000000000002220 ) ;
#14754 = EDGE_CURVE ( 'NONE', #7899, #14107, #1251, .T. ) ;
#14755 = CARTESIAN_POINT ( 'NONE',  ( -10.22290649399595353, 43.00645089659918341, 68.06527860057354928 ) ) ;
#14756 = ORIENTED_EDGE ( 'NONE', *, *, #12284, .T. ) ;
#14757 = EDGE_CURVE ( 'NONE', #14107, #18749, #2955, .T. ) ;
#14758 = EDGE_CURVE ( 'NONE', #6504, #8651, #20451, .T. ) ;
#14759 = VERTEX_POINT ( 'NONE', #6773 ) ;
#14760 = CARTESIAN_POINT ( 'NONE',  ( 25.37540678000427263, -66.94634676501046044, 13.50000000000000000 ) ) ;
#14761 = CONTEXT_DEPENDENT_SHAPE_REPRESENTATION ( #16001, #18962 ) ;
#14762 = ORIENTED_EDGE ( 'NONE', *, *, #8425, .T. ) ;
#14763 = CARTESIAN_POINT ( 'NONE',  ( 0.000000000000000000, 84.70000000000001705, 79.70000000000000284 ) ) ;
#14764 = CARTESIAN_POINT ( 'NONE',  ( 30.19999999999999574, 69.70000000000000284, 1.500000000000003997 ) ) ;
#14765 = DIRECTION ( 'NONE',  ( -0.000000000000000000, -1.000000000000000000, -0.000000000000000000 ) ) ;
#14766 = CYLINDRICAL_SURFACE ( 'NONE', #2008, 0.1000000000000028644 ) ;
#14767 = DIRECTION ( 'NONE',  ( 1.000000000000000000, 0.000000000000000000, 0.000000000000000000 ) ) ;
#14768 = LINE ( 'NONE', #15905, #13892 ) ;
#14769 = LINE ( 'NONE', #13206, #6844 ) ;
#14770 = FACE_OUTER_BOUND ( 'NONE', #4470, .T. ) ;
#14771 = CARTESIAN_POINT ( 'NONE',  ( 29.13662752439705272, 0.000000000000000000, 13.50000000000000000 ) ) ;
#14772 = CARTESIAN_POINT ( 'NONE',  ( 25.37540678000429395, -38.74634676501045760, 42.50000000000000000 ) ) ;
#14773 = EDGE_CURVE ( 'NONE', #21506, #799, #7590, .T. ) ;
#14774 = ORIENTED_EDGE ( 'NONE', *, *, #7022, .T. ) ;
#14775 = DIRECTION ( 'NONE',  ( 0.000000000000000000, 0.000000000000000000, 1.000000000000000000 ) ) ;
#14776 =( GEOMETRIC_REPRESENTATION_CONTEXT ( 3 ) GLOBAL_UNCERTAINTY_ASSIGNED_CONTEXT ( ( #8734 ) ) GLOBAL_UNIT_ASSIGNED_CONTEXT ( ( #6199, #3041, #1234 ) ) REPRESENTATION_CONTEXT ( 'NONE', 'WORKASPACE' ) );
#14777 = ADVANCED_FACE ( 'NONE', ( #13573 ), #20094, .T. ) ;
#14778 = DIRECTION ( 'NONE',  ( -3.290703158753225287E-15, 1.000000000000000000, 4.029949090311222146E-31 ) ) ;
#14779 = ORIENTED_EDGE ( 'NONE', *, *, #10020, .F. ) ;
#14780 = EDGE_LOOP ( 'NONE', ( #9874, #9797, #13244, #12350 ) ) ;
#14781 = CYLINDRICAL_SURFACE ( 'NONE', #7811, 0.05000000000000143219 ) ;
#14782 =( LENGTH_UNIT ( ) NAMED_UNIT ( * ) SI_UNIT ( .MILLI., .METRE. ) );
#14783 = ORIENTED_EDGE ( 'NONE', *, *, #10049, .T. ) ;
#14784 = CIRCLE ( 'NONE', #479, 0.1000000000000028644 ) ;
#14785 = VERTEX_POINT ( 'NONE', #5080 ) ;
#14786 = EDGE_LOOP ( 'NONE', ( #11644, #3046, #2308, #5658 ) ) ;
#14787 = CARTESIAN_POINT ( 'NONE',  ( -14.90262739788949098, -52.32122552996407450, 13.50000000000000000 ) ) ;
#14788 = AXIS2_PLACEMENT_3D ( 'NONE', #4715, #6740, #16783 ) ;
#14789 = EDGE_LOOP ( 'NONE', ( #20439, #21423, #12564, #8174 ) ) ;
#14790 = CYLINDRICAL_SURFACE ( 'NONE', #1998, 0.2999999999999999334 ) ;
#14791 = AXIS2_PLACEMENT_3D ( 'NONE', #19654, #4326, #17964 ) ;
#14792 = ORIENTED_EDGE ( 'NONE', *, *, #4443, .T. ) ;
#14793 = DIRECTION ( 'NONE',  ( -0.000000000000000000, -0.000000000000000000, -1.000000000000000000 ) ) ;
#14794 = SPHERICAL_SURFACE ( 'NONE', #18640, 0.5000000000000000000 ) ;
#14795 = DIRECTION ( 'NONE',  ( 1.000000000000000000, 0.000000000000000000, 0.000000000000000000 ) ) ;
#14796 = ADVANCED_FACE ( 'NONE', ( #5417 ), #19009, .F. ) ;
#14797 = ORIENTED_EDGE ( 'NONE', *, *, #17052, .T. ) ;
#14798 = CARTESIAN_POINT ( 'NONE',  ( -9.178906393579158163, 42.46645089659918426, 68.06527860057354928 ) ) ;
#14799 = EDGE_LOOP ( 'NONE', ( #14983, #12960, #5610, #1487 ) ) ;
#14800 = ORIENTED_EDGE ( 'NONE', *, *, #19738, .T. ) ;
#14801 = VERTEX_POINT ( 'NONE', #13891 ) ;
#14802 = CARTESIAN_POINT ( 'NONE',  ( 15.21174975910705918, 52.10286008774954780, 13.87500000000000000 ) ) ;
#14803 = DIRECTION ( 'NONE',  ( 1.000000000000000000, 0.000000000000000000, 0.000000000000000000 ) ) ;
#14804 = ORIENTED_EDGE ( 'NONE', *, *, #12703, .T. ) ;
#14805 = DIRECTION ( 'NONE',  ( -0.9729678061520339316, -0.2309407893632008379, 0.000000000000000000 ) ) ;
#14806 = CIRCLE ( 'NONE', #1222, 0.3000000000000000444 ) ;
#14807 = ORIENTED_EDGE ( 'NONE', *, *, #19646, .F. ) ;
#14808 = CARTESIAN_POINT ( 'NONE',  ( 29.37540678000427619, -6.000000000000000000, 3.799999999999999822 ) ) ;
#14809 = CARTESIAN_POINT ( 'NONE',  ( 15.95292532278785913, 34.11873716947361856, 68.50000000000000000 ) ) ;
#14810 = ADVANCED_FACE ( 'NONE', ( #10342 ), #15469, .F. ) ;
#14811 = CARTESIAN_POINT ( 'NONE',  ( -28.57540678000427548, 63.74634676501045050, 13.50000000000000000 ) ) ;
#14812 = DIRECTION ( 'NONE',  ( 0.000000000000000000, 0.000000000000000000, -1.000000000000000000 ) ) ;
#14813 = EDGE_LOOP ( 'NONE', ( #8223, #6496, #6589, #8463, #5286, #14004 ) ) ;
#14814 = CYLINDRICAL_SURFACE ( 'NONE', #15944, 0.5000000000000004441 ) ;
#14815 = DIRECTION ( 'NONE',  ( 0.000000000000000000, 0.000000000000000000, 1.000000000000000000 ) ) ;
#14816 = DIRECTION ( 'NONE',  ( 0.000000000000000000, 0.000000000000000000, 1.000000000000000000 ) ) ;
#14817 = VERTEX_POINT ( 'NONE', #20745 ) ;
#14818 = CARTESIAN_POINT ( 'NONE',  ( -29.69597781366221412, 27.99124249474150972, 68.75000000000000000 ) ) ;
#14819 = AXIS2_PLACEMENT_3D ( 'NONE', #20054, #1122, #13545 ) ;
#14820 = AXIS2_PLACEMENT_3D ( 'NONE', #13150, #4329, #16268 ) ;
#14821 = DIRECTION ( 'NONE',  ( -3.387630566026860322E-15, 1.000000000000000000, -1.333119110027185404E-17 ) ) ;
#14822 = ADVANCED_FACE ( 'NONE', ( #3621 ), #3178, .T. ) ;
#14823 = VERTEX_POINT ( 'NONE', #8665 ) ;
#14824 = CARTESIAN_POINT ( 'NONE',  ( 1.724728116533979616, 43.31054587065082728, 29.76679706732590702 ) ) ;
#14825 = EDGE_CURVE ( 'NONE', #7627, #3678, #12189, .T. ) ;
#14826 = LINE ( 'NONE', #16168, #5263 ) ;
#14827 = ORIENTED_EDGE ( 'NONE', *, *, #4745, .F. ) ;
#14828 = ORIENTED_EDGE ( 'NONE', *, *, #18754, .T. ) ;
#14829 = ORIENTED_EDGE ( 'NONE', *, *, #11541, .T. ) ;
#14830 = DIRECTION ( 'NONE',  ( -1.000000000000000000, 0.000000000000000000, 0.000000000000000000 ) ) ;
#14831 = EDGE_CURVE ( 'NONE', #7888, #2103, #18493, .T. ) ;
#14832 = DIRECTION ( 'NONE',  ( 0.000000000000000000, -1.000000000000000000, 0.000000000000000000 ) ) ;
#14833 = ORIENTED_EDGE ( 'NONE', *, *, #12229, .F. ) ;
#14834 = ORIENTED_EDGE ( 'NONE', *, *, #3347, .T. ) ;
#14835 = LINE ( 'NONE', #21693, #18979 ) ;
#14836 = CIRCLE ( 'NONE', #15547, 0.09999999999999939493 ) ;
#14837 = AXIS2_PLACEMENT_3D ( 'NONE', #3768, #10915, #11030 ) ;
#14838 = EDGE_CURVE ( 'NONE', #20113, #1398, #9344, .T. ) ;
#14839 = DIRECTION ( 'NONE',  ( 0.000000000000000000, 0.000000000000000000, -1.000000000000000000 ) ) ;
#14840 = LINE ( 'NONE', #11491, #16327 ) ;
#14841 = CARTESIAN_POINT ( 'NONE',  ( 14.37248138918699425, 42.46645089659917716, 70.50000000000000000 ) ) ;
#14842 = CARTESIAN_POINT ( 'NONE',  ( -24.69594744299175915, 42.46645089659918426, 68.50000000000000000 ) ) ;
#14843 = CARTESIAN_POINT ( 'NONE',  ( -18.22752199202934520, 50.11873716947361856, 13.50000000000000000 ) ) ;
#14844 = DIRECTION ( 'NONE',  ( -0.000000000000000000, -0.000000000000000000, -1.000000000000000000 ) ) ;
#14845 = DIRECTION ( 'NONE',  ( 1.000000000000000000, 0.000000000000000000, 0.000000000000000000 ) ) ;
#14846 = DIRECTION ( 'NONE',  ( -0.000000000000000000, 1.000000000000000000, -0.000000000000000000 ) ) ;
#14847 = VERTEX_POINT ( 'NONE', #5187 ) ;
#14848 = DIRECTION ( 'NONE',  ( 0.000000000000000000, 0.000000000000000000, -1.000000000000000000 ) ) ;
#14849 = AXIS2_PLACEMENT_3D ( 'NONE', #17019, #5068, #4418 ) ;
#14850 = ADVANCED_FACE ( 'NONE', ( #15562 ), #11989, .T. ) ;
#14851 = CARTESIAN_POINT ( 'NONE',  ( -30.79999999999999361, -84.70000000000001705, 9.999999999999998224 ) ) ;
#14852 = EDGE_LOOP ( 'NONE', ( #15160, #19608, #13579, #10898 ) ) ;
#14853 = CIRCLE ( 'NONE', #5234, 0.05000000000000143219 ) ;
#14854 = AXIS2_PLACEMENT_3D ( 'NONE', #8678, #20648, #15045 ) ;
#14856 = EDGE_CURVE ( 'NONE', #14913, #11183, #8426, .T. ) ;
#14855 = CYLINDRICAL_SURFACE ( 'NONE', #9972, 2.000000000000001776 ) ;
#14857 = PLANE ( 'NONE',  #6369 ) ;
#14858 = VERTEX_POINT ( 'NONE', #1485 ) ;
#14859 = VERTEX_POINT ( 'NONE', #15130 ) ;
#14860 = CARTESIAN_POINT ( 'NONE',  ( 29.50000000000002132, -2.473451120191013430, 0.2999999999999947153 ) ) ;
#14861 =( REPRESENTATION_RELATIONSHIP ('NONE','NONE', #561, #9142 ) REPRESENTATION_RELATIONSHIP_WITH_TRANSFORMATION ( #14316 )SHAPE_REPRESENTATION_RELATIONSHIP( ) );
#14862 = ORIENTED_EDGE ( 'NONE', *, *, #10767, .F. ) ;
#14863 = CIRCLE ( 'NONE', #3086, 0.04999999999999991257 ) ;
#14864 = CIRCLE ( 'NONE', #18809, 0.1000000000000028644 ) ;
#14865 = CARTESIAN_POINT ( 'NONE',  ( 27.61238352468048518, -2.348761424523157615, 0.000000000000000000 ) ) ;
#14866 = DIRECTION ( 'NONE',  ( -1.000000000000000000, 0.000000000000000000, 0.000000000000000000 ) ) ;
#14867 = VECTOR ( 'NONE', #11529, 1000.000000000000000 ) ;
#14868 = CYLINDRICAL_SURFACE ( 'NONE', #19504, 0.2500000000000002220 ) ;
#14869 = EDGE_CURVE ( 'NONE', #14314, #1350, #14703, .T. ) ;
#14870 = CARTESIAN_POINT ( 'NONE',  ( 15.95292532278785913, -50.11873716947361856, 68.00000000000000000 ) ) ;
#14871 = CARTESIAN_POINT ( 'NONE',  ( 23.02398829872513986, 3.419159475692122196, 13.52813170334708914 ) ) ;
#14872 = EDGE_CURVE ( 'NONE', #19359, #2691, #17037, .T. ) ;
#14873 = LINE ( 'NONE', #6409, #11059 ) ;
#14874 = CARTESIAN_POINT ( 'NONE',  ( 1.724728116533979616, 42.36054587065083155, 47.80876104995653719 ) ) ;
#14875 = DIRECTION ( 'NONE',  ( 0.000000000000000000, -0.000000000000000000, 1.000000000000000000 ) ) ;
#14876 = LINE ( 'NONE', #21403, #6526 ) ;
#14877 = AXIS2_PLACEMENT_3D ( 'NONE', #2190, #3996, #2519 ) ;
#14878 = CARTESIAN_POINT ( 'NONE',  ( -13.75390639357915923, 42.46645089659918426, 74.06027860057353962 ) ) ;
#14879 = AXIS2_PLACEMENT_3D ( 'NONE', #8573, #20650, #5206 ) ;
#14880 = VECTOR ( 'NONE', #15624, 1000.000000000000000 ) ;
#14881 = AXIS2_PLACEMENT_3D ( 'NONE', #17273, #5546, #3867 ) ;
#14882 = EDGE_CURVE ( 'NONE', #12488, #17779, #10078, .T. ) ;
#14883 = FACE_OUTER_BOUND ( 'NONE', #16409, .T. ) ;
#14884 = VERTEX_POINT ( 'NONE', #6987 ) ;
#14885 = DIRECTION ( 'NONE',  ( 0.000000000000000000, 0.000000000000000000, 1.000000000000000000 ) ) ;
#14886 = LINE ( 'NONE', #7750, #18135 ) ;
#14887 = ORIENTED_EDGE ( 'NONE', *, *, #2653, .F. ) ;
#14888 = AXIS2_PLACEMENT_3D ( 'NONE', #4779, #19778, #8251 ) ;
#14889 = ORIENTED_EDGE ( 'NONE', *, *, #20011, .F. ) ;
#14890 = CARTESIAN_POINT ( 'NONE',  ( 29.50000000000002132, 0.000000000000000000, 0.2999999999999947153 ) ) ;
#14891 = UNCERTAINTY_MEASURE_WITH_UNIT (LENGTH_MEASURE( 1.000000000000000082E-05 ), #19957, 'distance_accuracy_value', 'NONE');
#14892 = VERTEX_POINT ( 'NONE', #13772 ) ;
#14893 = ORIENTED_EDGE ( 'NONE', *, *, #4008, .T. ) ;
#14894 = ORIENTED_EDGE ( 'NONE', *, *, #16528, .T. ) ;
#14895 = AXIS2_PLACEMENT_3D ( 'NONE', #5430, #3969, #14238 ) ;
#14896 = AXIS2_PLACEMENT_3D ( 'NONE', #10071, #20367, #3458 ) ;
#14897 = TOROIDAL_SURFACE ( 'NONE', #20264, 0.05000000000000000278, 0.05000000000000000278 ) ;
#14898 = ORIENTED_EDGE ( 'NONE', *, *, #7093, .T. ) ;
#14899 = EDGE_CURVE ( 'NONE', #17668, #11071, #3285, .T. ) ;
#14900 = DIRECTION ( 'NONE',  ( -0.000000000000000000, -0.000000000000000000, 1.000000000000000000 ) ) ;
#14901 = AXIS2_PLACEMENT_3D ( 'NONE', #11016, #16382, #822 ) ;
#14902 = EDGE_CURVE ( 'NONE', #13226, #6000, #12427, .T. ) ;
#14903 = DIRECTION ( 'NONE',  ( 1.000000000000000000, 0.000000000000000000, 0.000000000000000000 ) ) ;
#14904 = ORIENTED_EDGE ( 'NONE', *, *, #7903, .F. ) ;
#14905 = CARTESIAN_POINT ( 'NONE',  ( 0.000000000000000000, 68.44634676501046044, 7.200000000000000178 ) ) ;
#14906 = DIRECTION ( 'NONE',  ( 0.000000000000000000, 0.000000000000000000, -1.000000000000000000 ) ) ;
#14907 = FACE_OUTER_BOUND ( 'NONE', #2646, .T. ) ;
#14908 = CARTESIAN_POINT ( 'NONE',  ( -1.774728116533986766, 42.31054587065082728, 16.00000000000000000 ) ) ;
#14909 = AXIS2_PLACEMENT_3D ( 'NONE', #16523, #6486, #13383 ) ;
#14910 = EDGE_LOOP ( 'NONE', ( #15166, #4511, #1541, #16644 ) ) ;
#14911 = AXIS2_PLACEMENT_3D ( 'NONE', #7057, #5148, #6848 ) ;
#14912 = AXIS2_PLACEMENT_3D ( 'NONE', #4697, #8053, #7846 ) ;
#14913 = VERTEX_POINT ( 'NONE', #10661 ) ;
#14914 = EDGE_LOOP ( 'NONE', ( #14640, #20838, #6296, #15740 ) ) ;
#14915 = FACE_OUTER_BOUND ( 'NONE', #18431, .T. ) ;
#14916 = DIRECTION ( 'NONE',  ( -0.000000000000000000, 1.000000000000000000, 0.000000000000000000 ) ) ;
#14917 = ORIENTED_EDGE ( 'NONE', *, *, #18276, .T. ) ;
#14918 = AXIS2_PLACEMENT_3D ( 'NONE', #9424, #16223, #900 ) ;
#14919 = EDGE_CURVE ( 'NONE', #22137, #1525, #8269, .T. ) ;
#14920 = DIRECTION ( 'NONE',  ( 0.5176069476490314791, -0.8556185176499236933, 0.000000000000000000 ) ) ;
#14921 = AXIS2_PLACEMENT_3D ( 'NONE', #8110, #929, #3061 ) ;
#14922 = AXIS2_PLACEMENT_3D ( 'NONE', #12339, #19195, #21410 ) ;
#14923 = VERTEX_POINT ( 'NONE', #3956 ) ;
#14924 = CARTESIAN_POINT ( 'NONE',  ( -33.20000000000000284, -84.70000000000001705, 1.800000000000000266 ) ) ;
#14925 = CARTESIAN_POINT ( 'NONE',  ( 1.774728116533979660, 42.31054587065082728, 41.66679706732590915 ) ) ;
#14926 = EDGE_CURVE ( 'NONE', #5550, #8429, #16850, .T. ) ;
#14927 = EDGE_CURVE ( 'NONE', #14671, #15347, #355, .T. ) ;
#14928 = CARTESIAN_POINT ( 'NONE',  ( -35.00000000000001421, -84.70000000000001705, 79.39999999999999147 ) ) ;
#14929 = CIRCLE ( 'NONE', #284, 0.04999999999999991257 ) ;
#14930 = AXIS2_PLACEMENT_3D ( 'NONE', #9956, #11728, #8617 ) ;
#14931 = CARTESIAN_POINT ( 'NONE',  ( -25.37540678000427263, -63.74634676501045050, 3.799999999999999822 ) ) ;
#14932 = ORIENTED_EDGE ( 'NONE', *, *, #20512, .T. ) ;
#14933 = CARTESIAN_POINT ( 'NONE',  ( 1.724728116533979616, 43.26054587065083012, 31.70876104995653932 ) ) ;
#14934 = DIRECTION ( 'NONE',  ( 0.000000000000000000, 0.000000000000000000, 1.000000000000000000 ) ) ;
#14935 = AXIS2_PLACEMENT_3D ( 'NONE', #19563, #12830, #12606 ) ;
#14936 = DIRECTION ( 'NONE',  ( 1.000000000000000000, 0.000000000000000000, 0.000000000000000000 ) ) ;
#14937 = LINE ( 'NONE', #9910, #16825 ) ;
#14938 = ORIENTED_EDGE ( 'NONE', *, *, #19465, .F. ) ;
#14939 = CARTESIAN_POINT ( 'NONE',  ( -1.724728116533986721, 43.31054587065082728, 47.70876104995654288 ) ) ;
#14940 = CIRCLE ( 'NONE', #20666, 1.000000000000000888 ) ;
#14941 = CARTESIAN_POINT ( 'NONE',  ( -33.20000000000001705, -84.70000000000001705, 78.20000000000000284 ) ) ;
#14942 = CIRCLE ( 'NONE', #9591, 0.5000000000000004441 ) ;
#14943 = ORIENTED_EDGE ( 'NONE', *, *, #6468, .F. ) ;
#14944 = CYLINDRICAL_SURFACE ( 'NONE', #11257, 0.5000000000000004441 ) ;
#14945 = DIRECTION ( 'NONE',  ( 0.000000000000000000, 1.000000000000000000, 0.000000000000000000 ) ) ;
#14946 = VERTEX_POINT ( 'NONE', #2149 ) ;
#14947 = ORIENTED_EDGE ( 'NONE', *, *, #17726, .F. ) ;
#14948 = ORIENTED_EDGE ( 'NONE', *, *, #11561, .T. ) ;
#14949 = CARTESIAN_POINT ( 'NONE',  ( -32.29156311937309454, 83.96304096052088539, 68.25000000000000000 ) ) ;
#14950 = EDGE_CURVE ( 'NONE', #2238, #12093, #17360, .T. ) ;
#14951 = DIRECTION ( 'NONE',  ( -0.000000000000000000, -0.000000000000000000, -1.000000000000000000 ) ) ;
#14952 = AXIS2_PLACEMENT_3D ( 'NONE', #11981, #21865, #5180 ) ;
#14953 = ORIENTED_EDGE ( 'NONE', *, *, #18857, .F. ) ;
#14954 = AXIS2_PLACEMENT_3D ( 'NONE', #14051, #15833, #15730 ) ;
#14955 = ORIENTED_EDGE ( 'NONE', *, *, #21073, .F. ) ;
#14956 = DIRECTION ( 'NONE',  ( 0.000000000000000000, 1.000000000000000000, 0.000000000000000000 ) ) ;
#14957 = VECTOR ( 'NONE', #3343, 1000.000000000000000 ) ;
#14958 = EDGE_CURVE ( 'NONE', #20211, #2381, #8876, .T. ) ;
#14959 = ADVANCED_FACE ( 'NONE', ( #1890 ), #8388, .T. ) ;
#14960 = DIRECTION ( 'NONE',  ( 0.000000000000000000, -1.000000000000000000, 0.000000000000000000 ) ) ;
#14961 = CARTESIAN_POINT ( 'NONE',  ( -23.02398829872513986, -2.502127083158335541, 13.57904421648012949 ) ) ;
#14962 = EDGE_CURVE ( 'NONE', #6081, #16612, #8628, .T. ) ;
#14963 = PLANE ( 'NONE',  #7397 ) ;
#14964 = DIRECTION ( 'NONE',  ( -1.000000000000000000, 0.000000000000000000, 0.000000000000000000 ) ) ;
#14965 = CARTESIAN_POINT ( 'NONE',  ( -34.40000000000001279, -84.70000000000001705, 79.39999999999999147 ) ) ;
#14966 = DIRECTION ( 'NONE',  ( -0.000000000000000000, -1.000000000000000000, 0.000000000000000000 ) ) ;
#14967 = VECTOR ( 'NONE', #16833, 1000.000000000000000 ) ;
#14968 = DIRECTION ( 'NONE',  ( 0.000000000000000000, -1.084202172485523564E-15, -1.000000000000000000 ) ) ;
#14969 = DIRECTION ( 'NONE',  ( 0.000000000000000000, -0.000000000000000000, -1.000000000000000000 ) ) ;
#14970 = ORIENTED_EDGE ( 'NONE', *, *, #20359, .T. ) ;
#14971 = TOROIDAL_SURFACE ( 'NONE', #22141, 0.5999999999999999778, 0.2999999999999999889 ) ;
#14972 = DIRECTION ( 'NONE',  ( 0.000000000000000000, -0.000000000000000000, -1.000000000000000000 ) ) ;
#14973 = EDGE_CURVE ( 'NONE', #5901, #1178, #12549, .T. ) ;
#14974 = AXIS2_PLACEMENT_3D ( 'NONE', #6343, #8341, #14815 ) ;
#14975 = CARTESIAN_POINT ( 'NONE',  ( 9.178906393579156386, 42.46645089659917716, 70.50000000000000000 ) ) ;
#14976 = CARTESIAN_POINT ( 'NONE',  ( 29.13662752439705272, 0.000000000000000000, 7.500000000000000000 ) ) ;
#14977 = VERTEX_POINT ( 'NONE', #10180 ) ;
#14978 = DIRECTION ( 'NONE',  ( 1.000000000000000000, 0.000000000000000000, 0.000000000000000000 ) ) ;
#14979 = AXIS2_PLACEMENT_3D ( 'NONE', #16084, #19686, #11168 ) ;
#14980 = EDGE_CURVE ( 'NONE', #2238, #12110, #5044, .T. ) ;
#14981 = CARTESIAN_POINT ( 'NONE',  ( -9.641460742840918030, 32.11873716947361856, 109.6002446535588319 ) ) ;
#14982 = VERTEX_POINT ( 'NONE', #15198 ) ;
#14983 = ORIENTED_EDGE ( 'NONE', *, *, #12768, .T. ) ;
#14984 = DIRECTION ( 'NONE',  ( 1.000000000000000000, 0.000000000000000000, 0.000000000000000000 ) ) ;
#14985 = EDGE_LOOP ( 'NONE', ( #21804, #9312, #2451, #20824 ) ) ;
#14986 = ADVANCED_FACE ( 'NONE', ( #10512 ), #20816, .F. ) ;
#14987 = DIRECTION ( 'NONE',  ( 1.000000000000000000, 0.000000000000000000, -0.000000000000000000 ) ) ;
#14988 = CIRCLE ( 'NONE', #7869, 0.3000000000000016542 ) ;
#14989 = ORIENTED_EDGE ( 'NONE', *, *, #17216, .F. ) ;
#14990 = FACE_OUTER_BOUND ( 'NONE', #1877, .T. ) ;
#14991 =( GEOMETRIC_REPRESENTATION_CONTEXT ( 3 ) GLOBAL_UNCERTAINTY_ASSIGNED_CONTEXT ( ( #2830 ) ) GLOBAL_UNIT_ASSIGNED_CONTEXT ( ( #18722, #3395, #8990 ) ) REPRESENTATION_CONTEXT ( 'NONE', 'WORKASPACE' ) );
#14992 = CIRCLE ( 'NONE', #7854, 0.9652499999999990532 ) ;
#14993 = ADVANCED_FACE ( 'NONE', ( #10080 ), #6158, .T. ) ;
#14994 = LINE ( 'NONE', #10179, #19860 ) ;
#14995 = ADVANCED_FACE ( 'NONE', ( #16992 ), #15435, .F. ) ;
#14996 = DIRECTION ( 'NONE',  ( 0.000000000000000000, -1.000000000000000000, 0.000000000000000000 ) ) ;
#14997 = CARTESIAN_POINT ( 'NONE',  ( 1.724728116533979616, 42.36054587065083155, 39.80876104995653719 ) ) ;
#14998 = DIRECTION ( 'NONE',  ( 0.000000000000000000, -1.000000000000000000, 0.000000000000000000 ) ) ;
#14999 = DIRECTION ( 'NONE',  ( -1.000000000000000000, -0.000000000000000000, 2.388292521039847891E-16 ) ) ;
#15000 = DIRECTION ( 'NONE',  ( -0.000000000000000000, -0.000000000000000000, 1.000000000000000000 ) ) ;
#15001 = CARTESIAN_POINT ( 'NONE',  ( -14.66895121610833463, -51.92349730072803027, 13.50000000000000000 ) ) ;
#15002 = CARTESIAN_POINT ( 'NONE',  ( 33.19999999999999574, -84.70000000000001705, 1.200000000000004174 ) ) ;
#15003 = CIRCLE ( 'NONE', #16442, 2.500000000000000444 ) ;
#15004 = EDGE_CURVE ( 'NONE', #10209, #6583, #108, .T. ) ;
#15005 = CARTESIAN_POINT ( 'NONE',  ( -23.49018890325625364, 45.04852366434393218, 68.50000000000000000 ) ) ;
#15006 = ORIENTED_EDGE ( 'NONE', *, *, #17986, .T. ) ;
#15007 = DIRECTION ( 'NONE',  ( -1.000000000000000000, 0.000000000000000000, 0.000000000000000000 ) ) ;
#15008 = VECTOR ( 'NONE', #16183, 1000.000000000000000 ) ;
#15009 = AXIS2_PLACEMENT_3D ( 'NONE', #6436, #18268, #11326 ) ;
#15010 = CYLINDRICAL_SURFACE ( 'NONE', #19581, 0.2999999999999999889 ) ;
#15011 = ORIENTED_EDGE ( 'NONE', *, *, #5029, .F. ) ;
#15012 = EDGE_LOOP ( 'NONE', ( #13219, #690, #9254, #5082 ) ) ;
#15013 = DIRECTION ( 'NONE',  ( 1.000000000000000000, 0.000000000000000000, 0.000000000000000000 ) ) ;
#15014 = EDGE_CURVE ( 'NONE', #18912, #11071, #6954, .T. ) ;
#15015 = ORIENTED_EDGE ( 'NONE', *, *, #20059, .F. ) ;
#15016 =( NAMED_UNIT ( * ) SI_UNIT ( $, .STERADIAN. ) SOLID_ANGLE_UNIT ( ) );
#15017 = ORIENTED_EDGE ( 'NONE', *, *, #446, .T. ) ;
#15018 = VERTEX_POINT ( 'NONE', #12066 ) ;
#15019 = ORIENTED_EDGE ( 'NONE', *, *, #2444, .F. ) ;
#15020 = ADVANCED_FACE ( 'NONE', ( #3589 ), #18288, .T. ) ;
#15021 = VECTOR ( 'NONE', #14531, 1000.000000000000114 ) ;
#15022 = CARTESIAN_POINT ( 'NONE',  ( 14.96174975910705918, -51.83053110199097091, 13.82013245744073160 ) ) ;
#15023 =( GEOMETRIC_REPRESENTATION_CONTEXT ( 3 ) GLOBAL_UNCERTAINTY_ASSIGNED_CONTEXT ( ( #18258 ) ) GLOBAL_UNIT_ASSIGNED_CONTEXT ( ( #13995, #8977, #19051 ) ) REPRESENTATION_CONTEXT ( 'NONE', 'WORKASPACE' ) );
#15024 = CARTESIAN_POINT ( 'NONE',  ( -3.127054932750481964, -32.93424481021354921, 68.50000000000000000 ) ) ;
#15025 = ORIENTED_EDGE ( 'NONE', *, *, #250, .F. ) ;
#15026 = DIRECTION ( 'NONE',  ( -0.000000000000000000, 1.000000000000000000, -0.000000000000000000 ) ) ;
#15027 = DIRECTION ( 'NONE',  ( 0.000000000000000000, 0.000000000000000000, 1.000000000000000000 ) ) ;
#15028 = DIRECTION ( 'NONE',  ( 1.000000000000000000, 0.000000000000000000, -0.000000000000000000 ) ) ;
#15029 = CARTESIAN_POINT ( 'NONE',  ( 9.178906393579156386, 42.46645089659917716, 69.50000000000000000 ) ) ;
#15030 = ORIENTED_EDGE ( 'NONE', *, *, #14020, .T. ) ;
#15031 = ORIENTED_EDGE ( 'NONE', *, *, #14486, .T. ) ;
#15032 = ORIENTED_EDGE ( 'NONE', *, *, #14008, .T. ) ;
#15033 = LINE ( 'NONE', #40, #18134 ) ;
#15034 = AXIS2_PLACEMENT_3D ( 'NONE', #19481, #15887, #9197 ) ;
#15036 = ADVANCED_FACE ( 'NONE', ( #17222 ), #5381, .T. ) ;
#15035 = CARTESIAN_POINT ( 'NONE',  ( -33.80000000000001847, -85.00000000000000000, 78.20000000000000284 ) ) ;
#15037 = ORIENTED_EDGE ( 'NONE', *, *, #9076, .F. ) ;
#15038 = AXIS2_PLACEMENT_3D ( 'NONE', #21400, #4376, #9751 ) ;
#15039 = ADVANCED_FACE ( 'NONE', ( #3468 ), #8837, .F. ) ;
#15040 = CYLINDRICAL_SURFACE ( 'NONE', #17008, 0.04999999999999991257 ) ;
#15041 = ORIENTED_EDGE ( 'NONE', *, *, #1442, .F. ) ;
#15042 = CARTESIAN_POINT ( 'NONE',  ( 1.774728116533979660, 43.31054587065082728, 45.66679706732590205 ) ) ;
#15043 = DIRECTION ( 'NONE',  ( 2.688368618483499901E-15, -1.000000000000000000, -3.292302023554010137E-31 ) ) ;
#15044 = VECTOR ( 'NONE', #2059, 1000.000000000000000 ) ;
#15045 = DIRECTION ( 'NONE',  ( 0.000000000000000000, 0.000000000000000000, -1.000000000000000000 ) ) ;
#15046 = VERTEX_POINT ( 'NONE', #6849 ) ;
#15047 = LINE ( 'NONE', #14933, #8831 ) ;
#15048 = CARTESIAN_POINT ( 'NONE',  ( 14.66174975910705847, -51.76873716947361714, 13.79999999999999893 ) ) ;
#15049 = VECTOR ( 'NONE', #16857, 1000.000000000000000 ) ;
#15050 = DIRECTION ( 'NONE',  ( 1.000000000000000000, 0.000000000000000000, 0.000000000000000000 ) ) ;
#15051 = FACE_OUTER_BOUND ( 'NONE', #5218, .T. ) ;
#15052 = VERTEX_POINT ( 'NONE', #12170 ) ;
#15053 = PRODUCT_DEFINITION ( 'UNKNOWN', '', #11207, #204 ) ;
#15054 = DIRECTION ( 'NONE',  ( 0.000000000000000000, 1.000000000000000000, 0.000000000000000000 ) ) ;
#15055 = ORIENTED_EDGE ( 'NONE', *, *, #19813, .F. ) ;
#15056 = FACE_OUTER_BOUND ( 'NONE', #12230, .T. ) ;
#15057 = AXIS2_PLACEMENT_3D ( 'NONE', #17933, #915, #12775 ) ;
#15058 = CYLINDRICAL_SURFACE ( 'NONE', #12022, 0.2999999999999999334 ) ;
#15059 = ORIENTED_EDGE ( 'NONE', *, *, #8974, .F. ) ;
#15060 = AXIS2_PLACEMENT_3D ( 'NONE', #11029, #16156, #4319 ) ;
#15061 = ORIENTED_EDGE ( 'NONE', *, *, #5955, .F. ) ;
#15062 = ORIENTED_EDGE ( 'NONE', *, *, #2538, .F. ) ;
#15063 = CARTESIAN_POINT ( 'NONE',  ( -26.61833302554978786, -9.663695060508651125, 13.79999999999999893 ) ) ;
#15064 = ADVANCED_FACE ( 'NONE', ( #15642 ), #13642, .F. ) ;
#15065 = AXIS2_PLACEMENT_3D ( 'NONE', #1821, #3175, #10001 ) ;
#15066 = CARTESIAN_POINT ( 'NONE',  ( -29.13662752439705272, 0.000000000000000000, 7.200000000000000178 ) ) ;
#15067 = VECTOR ( 'NONE', #16812, 1000.000000000000000 ) ;
#15068 = EDGE_LOOP ( 'NONE', ( #12438, #15685, #8027, #4645 ) ) ;
#15069 = ORIENTED_EDGE ( 'NONE', *, *, #22143, .T. ) ;
#15070 = ORIENTED_EDGE ( 'NONE', *, *, #9789, .T. ) ;
#15071 = DIRECTION ( 'NONE',  ( -0.000000000000000000, 1.000000000000000000, -0.000000000000000000 ) ) ;
#15072 = CARTESIAN_POINT ( 'NONE',  ( -14.96174975910705207, -32.10873716947361345, 13.05380965755523448 ) ) ;
#15073 = CARTESIAN_POINT ( 'NONE',  ( 1.724728116533979616, 42.31054587065082728, 35.80876104995653009 ) ) ;
#15074 = AXIS2_PLACEMENT_3D ( 'NONE', #4419, #14374, #6228 ) ;
#15075 = DIRECTION ( 'NONE',  ( 1.000000000000000000, 0.000000000000000000, 0.000000000000000000 ) ) ;
#15076 = LINE ( 'NONE', #21921, #1141 ) ;
#15077 = DIRECTION ( 'NONE',  ( 1.000000000000000000, -0.000000000000000000, -0.000000000000000000 ) ) ;
#15078 = VECTOR ( 'NONE', #4815, 1000.000000000000000 ) ;
#15079 = AXIS2_PLACEMENT_3D ( 'NONE', #916, #17241, #15773 ) ;
#15080 = FACE_OUTER_BOUND ( 'NONE', #3627, .T. ) ;
#15081 = CARTESIAN_POINT ( 'NONE',  ( 27.37540678000428684, -36.74634676501047181, 42.50000000000000000 ) ) ;
#15082 = ORIENTED_EDGE ( 'NONE', *, *, #11291, .F. ) ;
#15083 = CYLINDRICAL_SURFACE ( 'NONE', #8057, 5.000000000000000888 ) ;
#15084 = ORIENTED_EDGE ( 'NONE', *, *, #21884, .T. ) ;
#15085 = EDGE_CURVE ( 'NONE', #6210, #1592, #8674, .T. ) ;
#15086 = CARTESIAN_POINT ( 'NONE',  ( 30.19999999999999574, 69.70000000000000284, 0.3000000000000033751 ) ) ;
#15087 = VERTEX_POINT ( 'NONE', #20592 ) ;
#15088 = EDGE_CURVE ( 'NONE', #17645, #14671, #15966, .T. ) ;
#15089 = ORIENTED_EDGE ( 'NONE', *, *, #19365, .T. ) ;
#15090 = FACE_OUTER_BOUND ( 'NONE', #5731, .T. ) ;
#15091 = CIRCLE ( 'NONE', #9378, 0.3000000000000016542 ) ;
#15092 = AXIS2_PLACEMENT_3D ( 'NONE', #4327, #8925, #7360 ) ;
#15093 = EDGE_LOOP ( 'NONE', ( #20390, #17235, #8460, #9963 ) ) ;
#15094 = CARTESIAN_POINT ( 'NONE',  ( 1.824728116533979705, 43.26054587065083012, 53.66679706732590915 ) ) ;
#15095 = EDGE_LOOP ( 'NONE', ( #20552, #21897, #16899, #13575 ) ) ;
#15096 = DIRECTION ( 'NONE',  ( 1.000000000000000000, 0.000000000000000000, 0.000000000000000000 ) ) ;
#15097 = VECTOR ( 'NONE', #13766, 1000.000000000000000 ) ;
#15098 = LINE ( 'NONE', #18454, #6741 ) ;
#15099 = EDGE_CURVE ( 'NONE', #13059, #8047, #15784, .T. ) ;
#15100 = CARTESIAN_POINT ( 'NONE',  ( -1.774728116533986766, 42.31054587065082728, 24.00000000000000000 ) ) ;
#15101 = CARTESIAN_POINT ( 'NONE',  ( 1.824728116533979261, 43.31054587065082728, 31.80876104995653719 ) ) ;
#15102 = CARTESIAN_POINT ( 'NONE',  ( -15.05373532783226054, -52.39333378048836920, 13.50000000000000000 ) ) ;
#15103 = PLANE ( 'NONE',  #10189 ) ;
#15104 = ADVANCED_FACE ( 'NONE', ( #14074 ), #15750, .T. ) ;
#15105 = EDGE_CURVE ( 'NONE', #11974, #1458, #5091, .T. ) ;
#15106 = DIRECTION ( 'NONE',  ( 0.000000000000000000, 0.000000000000000000, -1.000000000000000000 ) ) ;
#15107 = ORIENTED_EDGE ( 'NONE', *, *, #14015, .T. ) ;
#15108 = LINE ( 'NONE', #13654, #18453 ) ;
#15109 = EDGE_CURVE ( 'NONE', #10741, #15111, #4121, .T. ) ;
#15110 = ORIENTED_EDGE ( 'NONE', *, *, #3341, .T. ) ;
#15111 = VERTEX_POINT ( 'NONE', #12502 ) ;
#15112 = CARTESIAN_POINT ( 'NONE',  ( -15.95292532278785913, 50.11873716947361856, 13.50000000000000000 ) ) ;
#15113 = ADVANCED_FACE ( 'NONE', ( #17876 ), #21038, .T. ) ;
#15114 = DIRECTION ( 'NONE',  ( 0.000000000000000000, 0.000000000000000000, 1.000000000000000000 ) ) ;
#15115 = ORIENTED_EDGE ( 'NONE', *, *, #6661, .T. ) ;
#15116 = SURFACE_STYLE_FILL_AREA ( #20504 ) ;
#15117 = ORIENTED_EDGE ( 'NONE', *, *, #15522, .F. ) ;
#15118 = EDGE_LOOP ( 'NONE', ( #20366, #16484, #14144, #11871 ) ) ;
#15119 = CARTESIAN_POINT ( 'NONE',  ( -14.71174975910705029, 51.61873716947361856, 13.50000000000000000 ) ) ;
#15120 = EDGE_CURVE ( 'NONE', #12990, #10522, #17767, .T. ) ;
#15121 = FACE_OUTER_BOUND ( 'NONE', #15218, .T. ) ;
#15122 = DIRECTION ( 'NONE',  ( 0.000000000000000000, 0.000000000000000000, -1.000000000000000000 ) ) ;
#15123 = ORIENTED_EDGE ( 'NONE', *, *, #14825, .F. ) ;
#15124 = DIRECTION ( 'NONE',  ( 1.000000000000000000, 0.000000000000000000, 0.000000000000000000 ) ) ;
#15125 = CARTESIAN_POINT ( 'NONE',  ( -30.49999999999998934, 69.70000000000001705, 0.2999999999999999334 ) ) ;
#15126 = DIRECTION ( 'NONE',  ( -0.000000000000000000, -0.000000000000000000, -1.000000000000000000 ) ) ;
#15127 = AXIS2_PLACEMENT_3D ( 'NONE', #4828, #16462, #1463 ) ;
#15128 = CYLINDRICAL_SURFACE ( 'NONE', #5181, 3.500000000000003109 ) ;
#15129 = ORIENTED_EDGE ( 'NONE', *, *, #18214, .T. ) ;
#15130 = CARTESIAN_POINT ( 'NONE',  ( -33.80000000000000426, 85.00000000000000000, 1.800000000000000266 ) ) ;
#15131 = EDGE_CURVE ( 'NONE', #2930, #16763, #3297, .T. ) ;
#15132 = VERTEX_POINT ( 'NONE', #755 ) ;
#15133 = VERTEX_POINT ( 'NONE', #423 ) ;
#15134 = ORIENTED_EDGE ( 'NONE', *, *, #3660, .T. ) ;
#15135 = DIRECTION ( 'NONE',  ( -6.123233995736764803E-17, 0.000000000000000000, 1.000000000000000000 ) ) ;
#15136 = ADVANCED_FACE ( 'NONE', ( #7607 ), #9053, .F. ) ;
#15137 = DIRECTION ( 'NONE',  ( 0.000000000000000000, -0.000000000000000000, -1.000000000000000000 ) ) ;
#15138 = ORIENTED_EDGE ( 'NONE', *, *, #11252, .F. ) ;
#15139 = DIRECTION ( 'NONE',  ( 0.000000000000000000, 0.000000000000000000, 1.000000000000000000 ) ) ;
#15140 = CIRCLE ( 'NONE', #845, 0.3000000000000004885 ) ;
#15141 = ORIENTED_EDGE ( 'NONE', *, *, #4647, .T. ) ;
#15142 = DIRECTION ( 'NONE',  ( 0.000000000000000000, 0.000000000000000000, -1.000000000000000000 ) ) ;
#15143 = TOROIDAL_SURFACE ( 'NONE', #21959, 0.5999999999999999778, 0.2999999999999999889 ) ;
#15144 = DIRECTION ( 'NONE',  ( 0.000000000000000000, 1.000000000000000000, 0.000000000000000000 ) ) ;
#15145 = CYLINDRICAL_SURFACE ( 'NONE', #4597, 0.3000000000000016542 ) ;
#15146 = PLANE ( 'NONE',  #19505 ) ;
#15147 = ORIENTED_EDGE ( 'NONE', *, *, #13327, .F. ) ;
#15148 = DIRECTION ( 'NONE',  ( -1.224646799147353207E-16, -1.000000000000000000, 0.000000000000000000 ) ) ;
#15149 = FACE_OUTER_BOUND ( 'NONE', #13917, .T. ) ;
#15150 = EDGE_CURVE ( 'NONE', #4677, #10017, #12605, .T. ) ;
#15151 = CARTESIAN_POINT ( 'NONE',  ( -8.641460742840918030, -33.93424481021354921, 68.00000000000000000 ) ) ;
#15152 = EDGE_CURVE ( 'NONE', #18983, #13328, #17232, .T. ) ;
#15153 = CARTESIAN_POINT ( 'NONE',  ( 31.50000000000002132, -71.00000000000001421, 1.800000000000000044 ) ) ;
#15154 = CARTESIAN_POINT ( 'NONE',  ( -15.95292532278785913, 32.11873716947361856, 109.6002446535588319 ) ) ;
#15155 = ORIENTED_EDGE ( 'NONE', *, *, #12243, .T. ) ;
#15156 = CARTESIAN_POINT ( 'NONE',  ( -1.824728116533986810, 43.31054587065082728, 39.80876104995653719 ) ) ;
#15157 = ORIENTED_EDGE ( 'NONE', *, *, #14701, .T. ) ;
#15158 = CARTESIAN_POINT ( 'NONE',  ( -27.37540678000427974, -5.683640910026986681, 13.79999999999999893 ) ) ;
#15159 = CARTESIAN_POINT ( 'NONE',  ( -1.824728116533986810, 42.36054587065083155, 47.70876104995654288 ) ) ;
#15160 = ORIENTED_EDGE ( 'NONE', *, *, #15398, .F. ) ;
#15161 = VERTEX_POINT ( 'NONE', #17440 ) ;
#15162 = ORIENTED_EDGE ( 'NONE', *, *, #493, .F. ) ;
#15163 = PLANE ( 'NONE',  #7058 ) ;
#15164 = EDGE_CURVE ( 'NONE', #513, #10145, #20468, .T. ) ;
#15165 = SPHERICAL_SURFACE ( 'NONE', #13216, 0.5000000000000000000 ) ;
#15166 = ORIENTED_EDGE ( 'NONE', *, *, #15622, .T. ) ;
#15167 = FACE_OUTER_BOUND ( 'NONE', #21007, .T. ) ;
#15168 = VERTEX_POINT ( 'NONE', #12710 ) ;
#15169 = EDGE_LOOP ( 'NONE', ( #10101, #3378, #10381, #2037 ) ) ;
#15170 = DIRECTION ( 'NONE',  ( 1.000000000000000000, 0.000000000000000000, 0.000000000000000000 ) ) ;
#15171 = DIRECTION ( 'NONE',  ( -0.000000000000000000, 0.000000000000000000, -1.000000000000000000 ) ) ;
#15172 = ORIENTED_EDGE ( 'NONE', *, *, #20828, .F. ) ;
#15173 = DIRECTION ( 'NONE',  ( -1.000000000000000000, 0.000000000000000000, 1.224646799147353207E-16 ) ) ;
#15174 = CARTESIAN_POINT ( 'NONE',  ( -30.19999999999999574, 69.70000000000001705, 0.2999999999999999334 ) ) ;
#15175 = DIRECTION ( 'NONE',  ( 0.000000000000000000, 0.000000000000000000, 1.000000000000000000 ) ) ;
#15176 = VECTOR ( 'NONE', #13889, 1000.000000000000000 ) ;
#15177 = DIRECTION ( 'NONE',  ( 1.000000000000000000, -1.038507728162729222E-16, -1.357958710150075923E-16 ) ) ;
#15178 = ORIENTED_EDGE ( 'NONE', *, *, #18492, .T. ) ;
#15179 = CARTESIAN_POINT ( 'NONE',  ( -14.96174975910705207, -41.81054587065082728, 13.79999999999999893 ) ) ;
#15180 = CARTESIAN_POINT ( 'NONE',  ( -11.70301280599631610, -2.777792850139019443, 13.50000000000000000 ) ) ;
#15181 = PRODUCT ( 'Front Plate', 'Front Plate', '', ( #17238 ) ) ;
#15182 = DIRECTION ( 'NONE',  ( 1.000000000000000000, -2.007781800899081911E-16, -1.224646799147353207E-16 ) ) ;
#15183 = VERTEX_POINT ( 'NONE', #19240 ) ;
#15184 = EDGE_CURVE ( 'NONE', #4642, #4089, #12571, .T. ) ;
#15185 = CARTESIAN_POINT ( 'NONE',  ( -31.69597781366222122, 58.94165929845684815, 68.75000000000000000 ) ) ;
#15186 = ORIENTED_EDGE ( 'NONE', *, *, #18918, .F. ) ;
#15187 = CARTESIAN_POINT ( 'NONE',  ( 15.21174975910705918, 41.81054587065082728, 13.75000000000000000 ) ) ;
#15188 = DIRECTION ( 'NONE',  ( -0.000000000000000000, -0.000000000000000000, 1.000000000000000000 ) ) ;
#15189 = AXIS2_PLACEMENT_3D ( 'NONE', #7230, #5342, #481 ) ;
#15190 = ORIENTED_EDGE ( 'NONE', *, *, #10349, .T. ) ;
#15191 = AXIS2_PLACEMENT_3D ( 'NONE', #17745, #5902, #21234 ) ;
#15192 = CARTESIAN_POINT ( 'NONE',  ( -35.00000000000000000, 85.00000000000000000, 1.500000000000000000 ) ) ;
#15193 = ORIENTED_EDGE ( 'NONE', *, *, #5319, .T. ) ;
#15194 = EDGE_CURVE ( 'NONE', #21063, #19665, #9383, .T. ) ;
#15195 = CARTESIAN_POINT ( 'NONE',  ( -15.21174975910705207, -51.61873716947361856, 68.00000000000000000 ) ) ;
#15196 = LINE ( 'NONE', #19121, #21729 ) ;
#15197 = CIRCLE ( 'NONE', #6278, 6.499999999999999112 ) ;
#15198 = CARTESIAN_POINT ( 'NONE',  ( -14.96174975910705207, 41.81054587065082728, 68.25000000000000000 ) ) ;
#15199 = EDGE_CURVE ( 'NONE', #14759, #17313, #15964, .T. ) ;
#15200 = CARTESIAN_POINT ( 'NONE',  ( 25.37540678000429395, -38.74634676501045760, 13.79999999999999893 ) ) ;
#15201 = CARTESIAN_POINT ( 'NONE',  ( -23.13310673709249343, 45.37789868843801599, 68.25000000000000000 ) ) ;
#15202 = DIRECTION ( 'NONE',  ( 0.000000000000000000, 0.000000000000000000, -1.000000000000000000 ) ) ;
#15203 = AXIS2_PLACEMENT_3D ( 'NONE', #5878, #4405, #11009 ) ;
#15204 = AXIS2_PLACEMENT_3D ( 'NONE', #18630, #1510, #18301 ) ;
#15205 = AXIS2_PLACEMENT_3D ( 'NONE', #19529, #4001, #16157 ) ;
#15206 = CARTESIAN_POINT ( 'NONE',  ( -14.96174975910705207, 51.61873716947361856, 68.25000000000000000 ) ) ;
#15207 = DIRECTION ( 'NONE',  ( -0.2309407893632007824, 0.9729678061520339316, 6.042045757235441622E-14 ) ) ;
#15208 = DIRECTION ( 'NONE',  ( 0.000000000000000000, -0.000000000000000000, 1.000000000000000000 ) ) ;
#15209 = CARTESIAN_POINT ( 'NONE',  ( 29.17540678000427690, 63.74634676501045050, 7.799999999999999822 ) ) ;
#15210 = DIRECTION ( 'NONE',  ( 0.000000000000000000, -1.000000000000000000, 0.000000000000000000 ) ) ;
#15211 = ORIENTED_EDGE ( 'NONE', *, *, #5661, .T. ) ;
#15212 = DIRECTION ( 'NONE',  ( -1.000000000000000000, 0.000000000000000000, 0.000000000000000000 ) ) ;
#15213 = AXIS2_PLACEMENT_3D ( 'NONE', #12250, #6708, #20463 ) ;
#15215 = CARTESIAN_POINT ( 'NONE',  ( -25.37540678000427263, -67.24634676501045760, 13.50000000000000000 ) ) ;
#15214 = AXIS2_PLACEMENT_3D ( 'NONE', #11122, #18048, #18285 ) ;
#15216 = ORIENTED_EDGE ( 'NONE', *, *, #18615, .F. ) ;
#15217 = VECTOR ( 'NONE', #20619, 1000.000000000000000 ) ;
#15218 = EDGE_LOOP ( 'NONE', ( #18657, #15876, #8004, #20830 ) ) ;
#15219 = DIRECTION ( 'NONE',  ( -1.000000000000000000, -0.000000000000000000, 2.388292521039847891E-16 ) ) ;
#15220 = SHAPE_DEFINITION_REPRESENTATION ( #9830, #7461 ) ;
#15221 = EDGE_CURVE ( 'NONE', #7730, #18586, #525, .T. ) ;
#15222 = EDGE_LOOP ( 'NONE', ( #9396, #20163, #2793, #8522 ) ) ;
#15223 = VECTOR ( 'NONE', #14114, 1000.000000000000000 ) ;
#15224 = ORIENTED_EDGE ( 'NONE', *, *, #4381, .T. ) ;
#15225 = EDGE_LOOP ( 'NONE', ( #3408, #4192, #12725, #9013 ) ) ;
#15226 = EDGE_CURVE ( 'NONE', #16467, #20699, #9161, .T. ) ;
#15227 = CARTESIAN_POINT ( 'NONE',  ( -30.67540678000428045, -63.74634676501045050, 3.799999999999999822 ) ) ;
#15228 = CARTESIAN_POINT ( 'NONE',  ( -29.13662752439705272, 5.000000000000000000, 7.200000000000000178 ) ) ;
#15229 = EDGE_CURVE ( 'NONE', #7335, #16887, #4570, .T. ) ;
#15230 = DIRECTION ( 'NONE',  ( 0.000000000000000000, 0.000000000000000000, -1.000000000000000000 ) ) ;
#15231 = VECTOR ( 'NONE', #15824, 1000.000000000000000 ) ;
#15232 = AXIS2_PLACEMENT_3D ( 'NONE', #18395, #13254, #16262 ) ;
#15233 = CIRCLE ( 'NONE', #1660, 0.6999999999999992895 ) ;
#15234 = LINE ( 'NONE', #11875, #21392 ) ;
#15235 = AXIS2_PLACEMENT_3D ( 'NONE', #9723, #1420, #11590 ) ;
#15236 = ORIENTED_EDGE ( 'NONE', *, *, #5123, .T. ) ;
#15237 = LINE ( 'NONE', #13565, #5764 ) ;
#15238 = ADVANCED_FACE ( 'NONE', ( #1307 ), #1192, .T. ) ;
#15239 = CARTESIAN_POINT ( 'NONE',  ( -23.02398829872513986, 3.264233419183502072, 13.78834712654929717 ) ) ;
#15240 = DIRECTION ( 'NONE',  ( 2.832483164223434527E-16, -1.000000000000000000, 0.000000000000000000 ) ) ;
#15241 = CARTESIAN_POINT ( 'NONE',  ( 3.127054932750481964, 32.61873716947361856, 109.6002446535588319 ) ) ;
#15242 = CIRCLE ( 'NONE', #19523, 4.351418481279137218 ) ;
#15243 = CARTESIAN_POINT ( 'NONE',  ( 1.724728116533979616, 43.31054587065082728, 33.76679706732591058 ) ) ;
#15244 = ORIENTED_EDGE ( 'NONE', *, *, #6996, .F. ) ;
#15245 = ORIENTED_EDGE ( 'NONE', *, *, #9780, .F. ) ;
#15246 = ORIENTED_EDGE ( 'NONE', *, *, #5403, .F. ) ;
#15247 = FACE_OUTER_BOUND ( 'NONE', #18111, .T. ) ;
#15248 = CARTESIAN_POINT ( 'NONE',  ( 29.37540678000427619, 4.700000000000000178, 3.500000000000000000 ) ) ;
#15249 = EDGE_CURVE ( 'NONE', #9143, #20684, #793, .T. ) ;
#15250 = AXIS2_PLACEMENT_3D ( 'NONE', #15378, #10785, #3736 ) ;
#15251 = AXIS2_PLACEMENT_3D ( 'NONE', #2802, #21939, #3021 ) ;
#15252 = CIRCLE ( 'NONE', #19924, 0.05000000000000143219 ) ;
#15253 = CARTESIAN_POINT ( 'NONE',  ( 1.724728116533979616, 42.36054587065083155, 31.80876104995653719 ) ) ;
#15254 = AXIS2_PLACEMENT_3D ( 'NONE', #11597, #14968, #20355 ) ;
#15255 = AXIS2_PLACEMENT_3D ( 'NONE', #9786, #4644, #13346 ) ;
#15256 = ORIENTED_EDGE ( 'NONE', *, *, #4274, .T. ) ;
#15257 = FACE_OUTER_BOUND ( 'NONE', #20120, .T. ) ;
#15258 = AXIS2_PLACEMENT_3D ( 'NONE', #20116, #11580, #12025 ) ;
#15259 = EDGE_CURVE ( 'NONE', #5867, #15111, #17926, .T. ) ;
#15260 = DIRECTION ( 'NONE',  ( -0.000000000000000000, 0.000000000000000000, -1.000000000000000000 ) ) ;
#15261 = EDGE_CURVE ( 'NONE', #11552, #1923, #13998, .T. ) ;
#15262 = FACE_OUTER_BOUND ( 'NONE', #20068, .T. ) ;
#15263 = ORIENTED_EDGE ( 'NONE', *, *, #12884, .F. ) ;
#15264 = FACE_OUTER_BOUND ( 'NONE', #2002, .T. ) ;
#15265 = EDGE_CURVE ( 'NONE', #11429, #7220, #16423, .T. ) ;
#15266 = CARTESIAN_POINT ( 'NONE',  ( -15.95292532278785913, 52.09333383871509682, 13.79999999999999893 ) ) ;
#15267 = DIRECTION ( 'NONE',  ( -0.000000000000000000, 1.000000000000000000, 0.000000000000000000 ) ) ;
#15268 = DIRECTION ( 'NONE',  ( 0.000000000000000000, -0.000000000000000000, 1.000000000000000000 ) ) ;
#15269 = ORIENTED_EDGE ( 'NONE', *, *, #5634, .T. ) ;
#15270 = CIRCLE ( 'NONE', #9559, 0.5000000000000004441 ) ;
#15271 = CARTESIAN_POINT ( 'NONE',  ( -35.00000000000000000, 84.70000000000001705, 1.200000000000000178 ) ) ;
#15272 = ORIENTED_EDGE ( 'NONE', *, *, #20574, .F. ) ;
#15273 = LINE ( 'NONE', #3205, #3765 ) ;
#15274 = CIRCLE ( 'NONE', #9566, 0.2499999999999977796 ) ;
#15275 = CARTESIAN_POINT ( 'NONE',  ( 32.20000000000001705, -71.00000000000001421, 3.200000000000000178 ) ) ;
#15276 = ORIENTED_EDGE ( 'NONE', *, *, #20507, .F. ) ;
#15277 = EDGE_LOOP ( 'NONE', ( #17892, #3926, #10546, #12265 ) ) ;
#15278 = AXIS2_PLACEMENT_3D ( 'NONE', #4194, #14034, #5555 ) ;
#15279 = ORIENTED_EDGE ( 'NONE', *, *, #4525, .T. ) ;
#15280 = CARTESIAN_POINT ( 'NONE',  ( -24.13662752439704917, 0.000000000000000000, 3.799999999999999822 ) ) ;
#15281 = CARTESIAN_POINT ( 'NONE',  ( 33.19999999999999574, 85.00000000000000000, 78.20000000000000284 ) ) ;
#15282 = VECTOR ( 'NONE', #17183, 1000.000000000000000 ) ;
#15283 = CARTESIAN_POINT ( 'NONE',  ( -9.141460742840918030, -33.43424481021354921, 42.50000000000000000 ) ) ;
#15284 =( BOUNDED_CURVE ( )  B_SPLINE_CURVE ( 3, ( #6118, #11229, #16253, #7790 ),
 .UNSPECIFIED., .F., .T. ) 
 B_SPLINE_CURVE_WITH_KNOTS ( ( 4, 4 ),
 ( 0.000000000000000000, 1.570796326794896558 ),
 .UNSPECIFIED. ) 
 CURVE ( )  GEOMETRIC_REPRESENTATION_ITEM ( )  RATIONAL_B_SPLINE_CURVE ( ( 1.000000000000000000, 0.8047378541243649375, 0.8047378541243649375, 1.000000000000000000 ) ) 
 REPRESENTATION_ITEM ( '' )  );
#15285 = ORIENTED_EDGE ( 'NONE', *, *, #10134, .F. ) ;
#15286 = DIRECTION ( 'NONE',  ( -0.000000000000000000, 0.000000000000000000, -1.000000000000000000 ) ) ;
#15287 = EDGE_CURVE ( 'NONE', #22112, #17384, #11389, .T. ) ;
#15288 = ORIENTED_EDGE ( 'NONE', *, *, #876, .T. ) ;
#15289 = VECTOR ( 'NONE', #3247, 1000.000000000000000 ) ;
#15290 = DIRECTION ( 'NONE',  ( 1.000000000000000000, -0.000000000000000000, 0.000000000000000000 ) ) ;
#15291 = CARTESIAN_POINT ( 'NONE',  ( -18.22752199202934520, -50.11873716947361856, 13.79999999999999893 ) ) ;
#15292 = VECTOR ( 'NONE', #15043, 1000.000000000000000 ) ;
#15293 = AXIS2_PLACEMENT_3D ( 'NONE', #7821, #14494, #6363 ) ;
#15294 = ORIENTED_EDGE ( 'NONE', *, *, #12758, .T. ) ;
#15295 = DIRECTION ( 'NONE',  ( 0.000000000000000000, 0.000000000000000000, 1.000000000000000000 ) ) ;
#15296 = DIRECTION ( 'NONE',  ( 0.000000000000000000, -1.000000000000000000, 0.000000000000000000 ) ) ;
#15297 = AXIS2_PLACEMENT_3D ( 'NONE', #8186, #3469, #8511 ) ;
#15298 = CARTESIAN_POINT ( 'NONE',  ( 1.724728116533979616, 42.36054587065083155, 45.76679706732590347 ) ) ;
#15299 = AXIS2_PLACEMENT_3D ( 'NONE', #5969, #12979, #800 ) ;
#15300 = DIRECTION ( 'NONE',  ( 0.000000000000000000, 0.000000000000000000, -1.000000000000000000 ) ) ;
#15301 = ORIENTED_EDGE ( 'NONE', *, *, #2564, .T. ) ;
#15302 = CARTESIAN_POINT ( 'NONE',  ( 23.02398829872513986, 3.053353875533147299, 13.54966661417621587 ) ) ;
#15303 = CIRCLE ( 'NONE', #13864, 0.09999999999999939493 ) ;
#15304 = EDGE_CURVE ( 'NONE', #15586, #19753, #18216, .T. ) ;
#15305 = CARTESIAN_POINT ( 'NONE',  ( -28.87540678000427619, 63.74634676501045050, 13.19999999999999929 ) ) ;
#15306 = APPLICATION_CONTEXT ( 'automotive_design' ) ;
#15307 = DIRECTION ( 'NONE',  ( 0.000000000000000000, 0.000000000000000000, -1.000000000000000000 ) ) ;
#15308 = CARTESIAN_POINT ( 'NONE',  ( 0.000000000000000000, 52.11873716947361856, 68.00000000000000000 ) ) ;
#15309 = ORIENTED_EDGE ( 'NONE', *, *, #4498, .F. ) ;
#15310 = CARTESIAN_POINT ( 'NONE',  ( -9.178906393579158163, 42.46645089659918426, 68.06527860057354928 ) ) ;
#15311 = CARTESIAN_POINT ( 'NONE',  ( -1.724728116533986721, 43.26054587065083012, 35.80876104995653009 ) ) ;
#15312 = AXIS2_PLACEMENT_3D ( 'NONE', #15576, #16016, #10882 ) ;
#15313 = CIRCLE ( 'NONE', #7112, 0.6000000000000033085 ) ;
#15314 = ORIENTED_EDGE ( 'NONE', *, *, #21424, .T. ) ;
#15315 = DIRECTION ( 'NONE',  ( 0.000000000000000000, 0.000000000000000000, -1.000000000000000000 ) ) ;
#15316 = DIRECTION ( 'NONE',  ( 0.000000000000000000, 0.000000000000000000, 1.000000000000000000 ) ) ;
#15317 = CIRCLE ( 'NONE', #657, 0.05000000000000143219 ) ;
#15318 = VECTOR ( 'NONE', #9446, 1000.000000000000000 ) ;
#15319 = VERTEX_POINT ( 'NONE', #14843 ) ;
#15320 = DIRECTION ( 'NONE',  ( 1.000000000000000000, 0.000000000000000000, -1.224646799147353207E-16 ) ) ;
#15321 = ADVANCED_FACE ( 'NONE', ( #16527 ), #14629, .F. ) ;
#15322 = ORIENTED_EDGE ( 'NONE', *, *, #1043, .T. ) ;
#15323 = ADVANCED_FACE ( 'NONE', ( #11594 ), #9942, .T. ) ;
#15324 = DIRECTION ( 'NONE',  ( -1.000000000000000000, -0.000000000000000000, -0.000000000000000000 ) ) ;
#15325 = ORIENTED_EDGE ( 'NONE', *, *, #27, .F. ) ;
#15326 = LINE ( 'NONE', #10178, #18126 ) ;
#15327 = DIRECTION ( 'NONE',  ( 1.000000000000000000, -2.832483164223420229E-16, 0.000000000000000000 ) ) ;
#15328 = CARTESIAN_POINT ( 'NONE',  ( 0.000000000000000000, 43.26054587065083012, 27.75876104995654003 ) ) ;
#15329 = AXIS2_PLACEMENT_3D ( 'NONE', #20760, #17169, #5437 ) ;
#15330 = CARTESIAN_POINT ( 'NONE',  ( 29.20000000000002061, -68.70000000000001705, 0.000000000000000000 ) ) ;
#15331 = AXIS2_PLACEMENT_3D ( 'NONE', #530, #5606, #20822 ) ;
#15332 = CARTESIAN_POINT ( 'NONE',  ( -29.69597781366221767, 56.94165929845684815, 68.50000000000000000 ) ) ;
#15333 = CARTESIAN_POINT ( 'NONE',  ( -14.75141515765153954, -52.14252004795846318, 13.50000000000000000 ) ) ;
#15335 = EDGE_CURVE ( 'NONE', #11905, #13059, #14743, .T. ) ;
#15334 = DIRECTION ( 'NONE',  ( 0.000000000000000000, -1.000000000000000000, 0.000000000000000000 ) ) ;
#15336 = ORIENTED_EDGE ( 'NONE', *, *, #9385, .T. ) ;
#15337 = CYLINDRICAL_SURFACE ( 'NONE', #9190, 0.2500000000000002220 ) ;
#15338 = DIRECTION ( 'NONE',  ( 0.000000000000000000, 0.000000000000000000, -1.000000000000000000 ) ) ;
#15339 = CARTESIAN_POINT ( 'NONE',  ( 34.39999999999998437, -84.70000000000001705, 80.00000000000000000 ) ) ;
#15340 = EDGE_LOOP ( 'NONE', ( #20065, #2259, #5648, #18136 ) ) ;
#15341 = EDGE_LOOP ( 'NONE', ( #18264, #17863, #15525, #2155 ) ) ;
#15342 = CARTESIAN_POINT ( 'NONE',  ( 14.71174975910705740, 51.61873716947361856, 14.00000000000000000 ) ) ;
#15343 = ADVANCED_FACE ( 'NONE', ( #21593 ), #21486, .T. ) ;
#15344 = EDGE_LOOP ( 'NONE', ( #15110, #12431, #21906, #21965 ) ) ;
#15345 = AXIS2_PLACEMENT_3D ( 'NONE', #20595, #15530, #20149 ) ;
#15346 = ORIENTED_EDGE ( 'NONE', *, *, #8333, .T. ) ;
#15347 = VERTEX_POINT ( 'NONE', #2899 ) ;
#15348 = CARTESIAN_POINT ( 'NONE',  ( 15.95292532278785913, 52.39333383871510108, 13.50000000000000000 ) ) ;
#15349 = CARTESIAN_POINT ( 'NONE',  ( 30.07540678000427548, 0.000000000000000000, 7.500000000000000000 ) ) ;
#15350 = CIRCLE ( 'NONE', #5456, 0.1000000000000028644 ) ;
#15351 = DIRECTION ( 'NONE',  ( -0.000000000000000000, -0.000000000000000000, 1.000000000000000000 ) ) ;
#15352 = PLANE ( 'NONE',  #6488 ) ;
#15353 = ADVANCED_FACE ( 'NONE', ( #9726 ), #10807, .F. ) ;
#15354 = AXIS2_PLACEMENT_3D ( 'NONE', #6490, #8263, #21920 ) ;
#15355 = MECHANICAL_DESIGN_GEOMETRIC_PRESENTATION_REPRESENTATION (  '', ( #338 ), #12832 ) ;
#15356 = DIRECTION ( 'NONE',  ( -3.052134192567367925E-16, -1.000000000000000000, 0.000000000000000000 ) ) ;
#15357 = VECTOR ( 'NONE', #16849, 1000.000000000000000 ) ;
#15358 = CARTESIAN_POINT ( 'NONE',  ( 4.127054932750481520, -33.43424481021354921, 13.50000000000000000 ) ) ;
#15359 = CYLINDRICAL_SURFACE ( 'NONE', #8756, 0.09999999999999939493 ) ;
#15360 = CARTESIAN_POINT ( 'NONE',  ( 14.66918480534031843, -51.92478805997374280, 13.49999999999999645 ) ) ;
#15361 = DIRECTION ( 'NONE',  ( -0.000000000000000000, -0.000000000000000000, -1.000000000000000000 ) ) ;
#15362 = VERTEX_POINT ( 'NONE', #16628 ) ;
#15363 = ORIENTED_EDGE ( 'NONE', *, *, #9838, .F. ) ;
#15364 = VERTEX_POINT ( 'NONE', #8264 ) ;
#15365 = DIRECTION ( 'NONE',  ( -1.000000000000000000, 0.000000000000000000, -0.000000000000000000 ) ) ;
#15366 = EDGE_CURVE ( 'NONE', #18983, #17660, #14724, .T. ) ;
#15367 = CARTESIAN_POINT ( 'NONE',  ( -29.42156627136959557, -2.562835948873662506, 0.09431749384236855216 ) ) ;
#15368 = EDGE_CURVE ( 'NONE', #12236, #8942, #15076, .T. ) ;
#15369 = ORIENTED_EDGE ( 'NONE', *, *, #16309, .F. ) ;
#15370 = EDGE_CURVE ( 'NONE', #1798, #11697, #19680, .T. ) ;
#15371 = DIRECTION ( 'NONE',  ( 1.000000000000000000, 0.000000000000000000, 0.000000000000000000 ) ) ;
#15372 = CIRCLE ( 'NONE', #714, 1.826718556943725202 ) ;
#15373 = CIRCLE ( 'NONE', #5752, 0.3000000000000016542 ) ;
#15374 = PRODUCT_DEFINITION_SHAPE ( 'NONE', 'NONE',  #22172 ) ;
#15375 = ORIENTED_EDGE ( 'NONE', *, *, #4807, .F. ) ;
#15376 = DIRECTION ( 'NONE',  ( 1.000000000000000000, 0.000000000000000000, -0.000000000000000000 ) ) ;
#15377 = B_SPLINE_CURVE_WITH_KNOTS ( 'NONE', 3,
 ( #7916, #16503, #21230, #7680, #6019, #1168, #6129, #2747 ),
 .UNSPECIFIED., .F., .F.,
 ( 4, 2, 2, 4 ),
 ( 0.000000000000000000, 0.0001191530424135532222, 0.0002383060848271064444, 0.0004766121696541957583 ),
 .UNSPECIFIED. ) ;
#15378 = CARTESIAN_POINT ( 'NONE',  ( 30.19999999999999574, 70.29999999999999716, 0.3000000000000033751 ) ) ;
#15379 = CARTESIAN_POINT ( 'NONE',  ( -1.724728116533986721, 43.31054587065082728, 37.76679706732590347 ) ) ;
#15380 = ORIENTED_EDGE ( 'NONE', *, *, #19179, .F. ) ;
#15381 = DIRECTION ( 'NONE',  ( -1.000000000000000000, 0.000000000000000000, 0.000000000000000000 ) ) ;
#15382 = DIRECTION ( 'NONE',  ( 0.000000000000000000, -0.000000000000000000, -1.000000000000000000 ) ) ;
#15383 = EDGE_CURVE ( 'NONE', #16243, #11811, #20683, .T. ) ;
#15384 = LINE ( 'NONE', #1845, #14967 ) ;
#15385 = CARTESIAN_POINT ( 'NONE',  ( 27.67540678000429111, -36.74634676501047181, 13.50000000000000000 ) ) ;
#15386 = EDGE_LOOP ( 'NONE', ( #13027, #1324, #14917, #11803 ) ) ;
#15387 = FACE_OUTER_BOUND ( 'NONE', #13430, .T. ) ;
#15388 = TOROIDAL_SURFACE ( 'NONE', #19325, 0.05000000000000000278, 0.05000000000000000278 ) ;
#15389 = ORIENTED_EDGE ( 'NONE', *, *, #15811, .T. ) ;
#15390 = DIRECTION ( 'NONE',  ( 0.000000000000000000, 0.000000000000000000, -1.000000000000000000 ) ) ;
#15391 = DIRECTION ( 'NONE',  ( 1.000000000000000000, -0.000000000000000000, 0.000000000000000000 ) ) ;
#15392 = CARTESIAN_POINT ( 'NONE',  ( 29.37573593128808369, -68.87573593128806237, -5.171888261068354354E-15 ) ) ;
#15393 = ORIENTED_EDGE ( 'NONE', *, *, #3620, .F. ) ;
#15394 = ORIENTED_EDGE ( 'NONE', *, *, #21300, .F. ) ;
#15395 = VERTEX_POINT ( 'NONE', #13508 ) ;
#15396 = CARTESIAN_POINT ( 'NONE',  ( 3.627054932750481964, -32.11873716947361856, 68.00000000000000000 ) ) ;
#15397 = DIRECTION ( 'NONE',  ( 1.000000000000000000, 0.000000000000000000, 0.000000000000000000 ) ) ;
#15398 = EDGE_CURVE ( 'NONE', #1902, #6717, #3673, .T. ) ;
#15399 = DIRECTION ( 'NONE',  ( -1.000000000000000000, 0.000000000000000000, 0.000000000000000000 ) ) ;
#15400 = EDGE_CURVE ( 'NONE', #17289, #12433, #90, .T. ) ;
#15401 = VERTEX_POINT ( 'NONE', #10387 ) ;
#15402 = CARTESIAN_POINT ( 'NONE',  ( 31.50000000000002132, 71.00000000000001421, 3.500000000000000000 ) ) ;
#15403 = EDGE_CURVE ( 'NONE', #14043, #21877, #15447, .T. ) ;
#15404 = VERTEX_POINT ( 'NONE', #16863 ) ;
#15405 = CARTESIAN_POINT ( 'NONE',  ( -9.718906393579157310, 43.51045099701597252, 68.06527860057354928 ) ) ;
#15406 = ORIENTED_EDGE ( 'NONE', *, *, #21287, .F. ) ;
#15407 = DIRECTION ( 'NONE',  ( -0.000000000000000000, -1.000000000000000000, -0.000000000000000000 ) ) ;
#15408 = TOROIDAL_SURFACE ( 'NONE', #8630, 0.05000000000000000278, 0.05000000000000000278 ) ;
#15409 = DIRECTION ( 'NONE',  ( -0.000000000000000000, -0.000000000000000000, -1.000000000000000000 ) ) ;
#15410 = DIRECTION ( 'NONE',  ( 0.000000000000000000, -1.000000000000000000, 0.000000000000000000 ) ) ;
#15411 = DIRECTION ( 'NONE',  ( 1.000000000000000000, 0.000000000000000000, -2.388292521039847891E-16 ) ) ;
#15412 = ORIENTED_EDGE ( 'NONE', *, *, #17963, .F. ) ;
#15413 = CARTESIAN_POINT ( 'NONE',  ( 23.20993114852208805, 3.065002284660069076, 13.47295189337469878 ) ) ;
#15414 = CARTESIAN_POINT ( 'NONE',  ( 0.000000000000000000, 42.31054587065082728, 47.75876104995653293 ) ) ;
#15415 = EDGE_CURVE ( 'NONE', #8431, #18168, #22152, .T. ) ;
#15416 = CARTESIAN_POINT ( 'NONE',  ( 29.69597781366221767, 27.99124249474150972, 70.25000000000000000 ) ) ;
#15417 = LINE ( 'NONE', #8371, #14593 ) ;
#15418 = VERTEX_POINT ( 'NONE', #11818 ) ;
#15419 = DIRECTION ( 'NONE',  ( -6.123233995736764803E-17, -0.000000000000000000, 1.000000000000000000 ) ) ;
#15420 = ADVANCED_FACE ( 'NONE', ( #10274 ), #6825, .T. ) ;
#15421 = CIRCLE ( 'NONE', #7569, 0.2999999999999947153 ) ;
#15422 = AXIS2_PLACEMENT_3D ( 'NONE', #11008, #480, #20979 ) ;
#15423 = EDGE_LOOP ( 'NONE', ( #13631, #9287, #13114, #6932 ) ) ;
#15424 = CARTESIAN_POINT ( 'NONE',  ( 24.13662752439704917, 0.000000000000000000, 7.500000000000000000 ) ) ;
#15425 = FACE_OUTER_BOUND ( 'NONE', #20397, .T. ) ;
#15426 = ORIENTED_EDGE ( 'NONE', *, *, #11565, .F. ) ;
#15427 = CARTESIAN_POINT ( 'NONE',  ( -1.724728116533986721, 43.26054587065083012, 33.71679706732589921 ) ) ;
#15428 = EDGE_CURVE ( 'NONE', #10963, #1577, #13620, .T. ) ;
#15429 = ORIENTED_EDGE ( 'NONE', *, *, #20167, .T. ) ;
#15430 = CIRCLE ( 'NONE', #11493, 5.000000000000000888 ) ;
#15431 = VECTOR ( 'NONE', #19275, 1000.000000000000000 ) ;
#15432 = DIRECTION ( 'NONE',  ( -0.000000000000000000, -0.000000000000000000, -1.000000000000000000 ) ) ;
#15433 = ORIENTED_EDGE ( 'NONE', *, *, #7645, .T. ) ;
#15434 = FACE_OUTER_BOUND ( 'NONE', #20506, .T. ) ;
#15435 = CYLINDRICAL_SURFACE ( 'NONE', #6881, 0.2999999999999999334 ) ;
#15436 = CARTESIAN_POINT ( 'NONE',  ( 25.37540678000426908, 38.74634676501045760, 42.50000000000000000 ) ) ;
#15437 = DIRECTION ( 'NONE',  ( 0.000000000000000000, 1.000000000000000000, 0.000000000000000000 ) ) ;
#15438 = EDGE_CURVE ( 'NONE', #20293, #16692, #1531, .T. ) ;
#15439 = CARTESIAN_POINT ( 'NONE',  ( 0.000000000000000000, 0.000000000000000000, 68.50000000000000000 ) ) ;
#15440 = EDGE_CURVE ( 'NONE', #8303, #6460, #1869, .T. ) ;
#15441 = CARTESIAN_POINT ( 'NONE',  ( -9.141460742840918030, 33.43424481021354921, 42.50000000000000000 ) ) ;
#15442 = EDGE_CURVE ( 'NONE', #9924, #14817, #8785, .T. ) ;
#15443 = ORIENTED_EDGE ( 'NONE', *, *, #6618, .F. ) ;
#15444 = CIRCLE ( 'NONE', #420, 0.1000000000000028644 ) ;
#15445 = CARTESIAN_POINT ( 'NONE',  ( 17.93704824106378837, -38.74634676501045760, 13.87500000000000000 ) ) ;
#15446 = DIRECTION ( 'NONE',  ( 2.107255972849994642E-16, 0.000000000000000000, 1.000000000000000000 ) ) ;
#15447 = CIRCLE ( 'NONE', #5822, 0.2500000000000002220 ) ;
#15448 = LINE ( 'NONE', #6965, #19485 ) ;
#15449 = ORIENTED_EDGE ( 'NONE', *, *, #12984, .T. ) ;
#15450 = ORIENTED_EDGE ( 'NONE', *, *, #546, .T. ) ;
#15451 = CARTESIAN_POINT ( 'NONE',  ( -1.724728116533986721, 42.36054587065083155, 45.66679706732590205 ) ) ;
#15452 =( NAMED_UNIT ( * ) SI_UNIT ( $, .STERADIAN. ) SOLID_ANGLE_UNIT ( ) );
#15453 = VERTEX_POINT ( 'NONE', #5241 ) ;
#15454 =( NAMED_UNIT ( * ) PLANE_ANGLE_UNIT ( ) SI_UNIT ( $, .RADIAN. ) );
#15455 = VECTOR ( 'NONE', #4154, 1000.000000000000000 ) ;
#15456 = EDGE_LOOP ( 'NONE', ( #8937, #7468, #77, #70 ) ) ;
#15457 = PRODUCT_RELATED_PRODUCT_CATEGORY ( 'part', '', ( #16590 ) ) ;
#15458 = ORIENTED_EDGE ( 'NONE', *, *, #18114, .T. ) ;
#15459 = DIRECTION ( 'NONE',  ( 1.000000000000000000, 0.000000000000000000, 0.000000000000000000 ) ) ;
#15460 = DIRECTION ( 'NONE',  ( 0.000000000000000000, -1.000000000000000000, 0.000000000000000000 ) ) ;
#15461 = CARTESIAN_POINT ( 'NONE',  ( -9.178906393579156386, 42.46645089659917716, 69.50000000000000000 ) ) ;
#15462 = DIRECTION ( 'NONE',  ( -0.000000000000000000, 1.000000000000000000, -0.000000000000000000 ) ) ;
#15463 = EDGE_CURVE ( 'NONE', #3489, #4495, #3059, .T. ) ;
#15464 = CARTESIAN_POINT ( 'NONE',  ( -14.37248138918699425, 42.46645089659917716, 69.50000000000000000 ) ) ;
#15465 = CARTESIAN_POINT ( 'NONE',  ( -9.141460742840918030, 32.61873716947361856, 7.321391277662001151 ) ) ;
#15466 = ADVANCED_FACE ( 'NONE', ( #15505 ), #3333, .T. ) ;
#15467 = CARTESIAN_POINT ( 'NONE',  ( -15.21174975910705207, -51.86873716947361856, 13.05380965755523448 ) ) ;
#15468 = CARTESIAN_POINT ( 'NONE',  ( -1.724728116533986721, 43.31054587065082728, 35.75876104995654003 ) ) ;
#15469 = CYLINDRICAL_SURFACE ( 'NONE', #5431, 6.500000000000002665 ) ;
#15470 = EDGE_LOOP ( 'NONE', ( #4041, #3710, #3342, #15123 ) ) ;
#15471 = ORIENTED_EDGE ( 'NONE', *, *, #14427, .T. ) ;
#15472 = CARTESIAN_POINT ( 'NONE',  ( -1.824728116533986810, 43.26054587065083012, 41.66679706732590915 ) ) ;
#15473 = DIRECTION ( 'NONE',  ( 0.000000000000000000, 1.000000000000000000, 0.000000000000000000 ) ) ;
#15474 = ORIENTED_EDGE ( 'NONE', *, *, #19492, .T. ) ;
#15475 = ORIENTED_EDGE ( 'NONE', *, *, #3199, .T. ) ;
#15476 = EDGE_CURVE ( 'NONE', #16066, #17364, #11621, .T. ) ;
#15477 = FACE_OUTER_BOUND ( 'NONE', #14342, .T. ) ;
#15478 = MECHANICAL_DESIGN_GEOMETRIC_PRESENTATION_REPRESENTATION (  '', ( #9778 ), #14776 ) ;
#15479 = DIRECTION ( 'NONE',  ( 0.000000000000000000, 0.000000000000000000, 1.000000000000000000 ) ) ;
#15480 = ORIENTED_EDGE ( 'NONE', *, *, #9152, .F. ) ;
#15481 = CARTESIAN_POINT ( 'NONE',  ( 28.87540678000427619, -63.74634676501045050, 13.19999999999999929 ) ) ;
#15482 = DIRECTION ( 'NONE',  ( -2.107255972849994642E-16, 0.000000000000000000, -1.000000000000000000 ) ) ;
#15483 = EDGE_CURVE ( 'NONE', #21353, #18406, #6286, .T. ) ;
#15484 = DIRECTION ( 'NONE',  ( 0.000000000000000000, -1.000000000000000000, 0.000000000000000000 ) ) ;
#15485 = CARTESIAN_POINT ( 'NONE',  ( 30.37540678000427619, 6.000000000000000000, 3.499999999999999556 ) ) ;
#15486 = SURFACE_STYLE_USAGE ( .BOTH. , #10132 ) ;
#15487 = PLANE ( 'NONE',  #552 ) ;
#15488 = FACE_OUTER_BOUND ( 'NONE', #15386, .T. ) ;
#15489 = DIRECTION ( 'NONE',  ( 1.000000000000000000, 0.000000000000000000, 0.000000000000000000 ) ) ;
#15490 = CARTESIAN_POINT ( 'NONE',  ( 29.13662752439705272, -4.700000000000000178, 3.799999999999999822 ) ) ;
#15491 = B_SPLINE_CURVE_WITH_KNOTS ( 'NONE', 3,
 ( #21756, #21301, #1140, #4173, #11440, #14787, #9772, #12769 ),
 .UNSPECIFIED., .F., .F.,
 ( 4, 2, 2, 4 ),
 ( 0.000000000000000000, 0.0002312589012449784136, 0.0004625178024899568273, 0.0009250356049798978252 ),
 .UNSPECIFIED. ) ;
#15492 = VERTEX_POINT ( 'NONE', #1962 ) ;
#15493 = VERTEX_POINT ( 'NONE', #1765 ) ;
#15494 = DIRECTION ( 'NONE',  ( -1.000000000000000000, 3.009265538104883829E-28, -4.336808689941893885E-15 ) ) ;
#15495 = DIRECTION ( 'NONE',  ( 0.000000000000000000, -1.000000000000000000, 0.000000000000000000 ) ) ;
#15496 = DIRECTION ( 'NONE',  ( 0.000000000000000000, 0.000000000000000000, -1.000000000000000000 ) ) ;
#15497 = ADVANCED_FACE ( 'NONE', ( #6200 ), #695, .F. ) ;
#15498 = EDGE_CURVE ( 'NONE', #11552, #9562, #12679, .T. ) ;
#15499 = ORIENTED_EDGE ( 'NONE', *, *, #17904, .T. ) ;
#15500 = CARTESIAN_POINT ( 'NONE',  ( -31.44597781366220701, -6.622080232047910987E-15, 68.50000000000000000 ) ) ;
#15501 = ORIENTED_EDGE ( 'NONE', *, *, #2668, .F. ) ;
#15502 = CARTESIAN_POINT ( 'NONE',  ( -19.16037735075775217, 42.46645089659918426, 13.74999999999999822 ) ) ;
#15503 = CARTESIAN_POINT ( 'NONE',  ( 29.13662752439705272, 0.000000000000000000, 13.19999999999999929 ) ) ;
#15504 = DIRECTION ( 'NONE',  ( 0.000000000000000000, 0.000000000000000000, -1.000000000000000000 ) ) ;
#15505 = FACE_OUTER_BOUND ( 'NONE', #15942, .T. ) ;
#15506 = ORIENTED_EDGE ( 'NONE', *, *, #4858, .T. ) ;
#15507 = CYLINDRICAL_SURFACE ( 'NONE', #12342, 4.575000000000001066 ) ;
#15508 = SPHERICAL_SURFACE ( 'NONE', #6407, 0.2999999999999999889 ) ;
#15509 = ADVANCED_FACE ( 'NONE', ( #6931 ), #4132, .T. ) ;
#15510 = EDGE_CURVE ( 'NONE', #10209, #15362, #2337, .T. ) ;
#15511 = CARTESIAN_POINT ( 'NONE',  ( 15.95292532278785913, 50.11873716947361856, 68.50000000000000000 ) ) ;
#15512 = DIRECTION ( 'NONE',  ( 0.000000000000000000, 0.000000000000000000, -1.000000000000000000 ) ) ;
#15513 = EDGE_LOOP ( 'NONE', ( #17614, #13625, #5135, #17282 ) ) ;
#15514 = CARTESIAN_POINT ( 'NONE',  ( -8.299557710647819775, 43.00645089659919051, 69.00503344894293889 ) ) ;
#15515 = EDGE_CURVE ( 'NONE', #19461, #21526, #10591, .T. ) ;
#15516 = DIRECTION ( 'NONE',  ( 0.000000000000000000, 0.000000000000000000, 1.000000000000000000 ) ) ;
#15517 = ORIENTED_EDGE ( 'NONE', *, *, #6830, .F. ) ;
#15518 = CARTESIAN_POINT ( 'NONE',  ( -29.37540678000427619, 5.299999999999999822, 7.500000000000000000 ) ) ;
#15519 = DIRECTION ( 'NONE',  ( -1.000000000000000000, 0.000000000000000000, 0.000000000000000000 ) ) ;
#15520 = ORIENTED_EDGE ( 'NONE', *, *, #1205, .T. ) ;
#15521 = ORIENTED_EDGE ( 'NONE', *, *, #7601, .T. ) ;
#15522 = EDGE_CURVE ( 'NONE', #8649, #2930, #501, .T. ) ;
#15523 = ORIENTED_EDGE ( 'NONE', *, *, #11504, .T. ) ;
#15524 = AXIS2_PLACEMENT_3D ( 'NONE', #20412, #16811, #6651 ) ;
#15525 = ORIENTED_EDGE ( 'NONE', *, *, #2653, .T. ) ;
#15526 = CARTESIAN_POINT ( 'NONE',  ( -29.50000000000002132, 2.473451120191013430, 0.2999999999999947153 ) ) ;
#15527 = CARTESIAN_POINT ( 'NONE',  ( -8.638906393579159015, 43.51045099701597252, 68.06527860057354928 ) ) ;
#15528 = CARTESIAN_POINT ( 'NONE',  ( -3.627054932750481964, 33.43424481021354921, 68.00000000000000000 ) ) ;
#15529 = EDGE_CURVE ( 'NONE', #12670, #3289, #19099, .T. ) ;
#15530 = DIRECTION ( 'NONE',  ( -0.000000000000000000, 0.000000000000000000, 1.000000000000000000 ) ) ;
#15531 = ADVANCED_FACE ( 'NONE', ( #397 ), #9855, .T. ) ;
#15532 = FACE_OUTER_BOUND ( 'NONE', #20672, .T. ) ;
#15533 = CARTESIAN_POINT ( 'NONE',  ( 14.96174975910705918, 42.31054587065082728, 13.75000000000000000 ) ) ;
#15534 = VECTOR ( 'NONE', #12813, 1000.000000000000000 ) ;
#15535 = AXIS2_PLACEMENT_3D ( 'NONE', #20573, #7040, #12479 ) ;
#15536 = ORIENTED_EDGE ( 'NONE', *, *, #17518, .T. ) ;
#15537 = DIRECTION ( 'NONE',  ( 1.000000000000000000, 0.000000000000000000, 0.000000000000000000 ) ) ;
#15538 = ORIENTED_EDGE ( 'NONE', *, *, #14610, .T. ) ;
#15539 = ORIENTED_EDGE ( 'NONE', *, *, #13523, .T. ) ;
#15540 = DIRECTION ( 'NONE',  ( 0.000000000000000000, 0.000000000000000000, 1.000000000000000000 ) ) ;
#15541 = APPLICATION_PROTOCOL_DEFINITION ( 'draft international standard', 'automotive_design', 1998, #5 ) ;
#15542 = EDGE_LOOP ( 'NONE', ( #12056, #37, #3202, #14318 ) ) ;
#15543 = AXIS2_PLACEMENT_3D ( 'NONE', #15291, #19697, #2580 ) ;
#15544 = ADVANCED_FACE ( 'NONE', ( #21006 ), #18799, .T. ) ;
#15545 = CARTESIAN_POINT ( 'NONE',  ( 23.02398829872514696, -2.388718329487954595, 13.39778868030486869 ) ) ;
#15546 = ORIENTED_EDGE ( 'NONE', *, *, #1445, .T. ) ;
#15547 = AXIS2_PLACEMENT_3D ( 'NONE', #8788, #3748, #15588 ) ;
#15548 = CIRCLE ( 'NONE', #5933, 0.1000000000000028644 ) ;
#15549 = EDGE_LOOP ( 'NONE', ( #9171, #63, #6216, #6826 ) ) ;
#15550 = DIRECTION ( 'NONE',  ( 0.000000000000000000, 1.000000000000000000, 0.000000000000000000 ) ) ;
#15551 = CARTESIAN_POINT ( 'NONE',  ( 34.99999999999999289, -84.70000000000001705, 0.6000000000000033085 ) ) ;
#15552 = CARTESIAN_POINT ( 'NONE',  ( -21.92816239687475743, 42.46645089659918426, 68.50000000000000000 ) ) ;
#15553 = CARTESIAN_POINT ( 'NONE',  ( 1.724728116533979838, 43.31054587065082728, 53.66679706732590915 ) ) ;
#15554 = CYLINDRICAL_SURFACE ( 'NONE', #8622, 2.000000000000001776 ) ;
#15555 = EDGE_CURVE ( 'NONE', #12963, #10963, #5217, .T. ) ;
#15556 = CARTESIAN_POINT ( 'NONE',  ( -23.02398829872513986, 2.157133568460911199, 13.19999999999998685 ) ) ;
#15557 = CYLINDRICAL_SURFACE ( 'NONE', #2217, 0.3000000000000016542 ) ;
#15558 = DIRECTION ( 'NONE',  ( -1.000000000000000000, 0.000000000000000000, 0.000000000000000000 ) ) ;
#15559 = CARTESIAN_POINT ( 'NONE',  ( 15.21174975910705918, 42.11054587065083155, 13.79999999999999893 ) ) ;
#15560 = AXIS2_PLACEMENT_3D ( 'NONE', #5030, #1432, #8168 ) ;
#15561 = AXIS2_PLACEMENT_3D ( 'NONE', #17472, #2019, #6978 ) ;
#15562 = FACE_OUTER_BOUND ( 'NONE', #4662, .T. ) ;
#15563 = VECTOR ( 'NONE', #9556, 1000.000000000000114 ) ;
#15564 = ORIENTED_EDGE ( 'NONE', *, *, #13436, .F. ) ;
#15565 = AXIS2_PLACEMENT_3D ( 'NONE', #20861, #5657, #7323 ) ;
#15566 = EDGE_LOOP ( 'NONE', ( #18535, #4362 ) ) ;
#15567 = LINE ( 'NONE', #1925, #5676 ) ;
#15568 = FACE_OUTER_BOUND ( 'NONE', #20060, .T. ) ;
#15569 = VERTEX_POINT ( 'NONE', #12472 ) ;
#15570 = ADVANCED_FACE ( 'NONE', ( #17734 ), #19210, .T. ) ;
#15571 = ADVANCED_FACE ( 'NONE', ( #19321 ), #619, .F. ) ;
#15572 = CIRCLE ( 'NONE', #4501, 0.2999999999999947153 ) ;
#15573 = VECTOR ( 'NONE', #14945, 1000.000000000000000 ) ;
#15574 = VECTOR ( 'NONE', #5155, 1000.000000000000000 ) ;
#15575 = DIRECTION ( 'NONE',  ( -0.000000000000000000, 0.000000000000000000, 1.000000000000000000 ) ) ;
#15576 = CARTESIAN_POINT ( 'NONE',  ( 33.19999999999999574, 85.00000000000000000, 1.799999999999996048 ) ) ;
#15577 = FACE_OUTER_BOUND ( 'NONE', #6393, .T. ) ;
#15578 = AXIS2_PLACEMENT_3D ( 'NONE', #12752, #5857, #2820 ) ;
#15579 = VERTEX_POINT ( 'NONE', #5895 ) ;
#15580 = CARTESIAN_POINT ( 'NONE',  ( -29.13662752439705272, -4.700000000000000178, 3.500000000000000000 ) ) ;
#15581 = DIRECTION ( 'NONE',  ( -1.000000000000000000, 0.000000000000000000, 0.000000000000000000 ) ) ;
#15582 = CARTESIAN_POINT ( 'NONE',  ( -1.724728116533986721, 43.31054587065082728, 39.80876104995653719 ) ) ;
#15583 = CARTESIAN_POINT ( 'NONE',  ( 25.37540678000427263, -68.44634676501046044, 7.500000000000000000 ) ) ;
#15584 = CARTESIAN_POINT ( 'NONE',  ( -9.178906393579158163, 42.46645089659918426, 74.06027860057353962 ) ) ;
#15585 = CARTESIAN_POINT ( 'NONE',  ( -14.66174975910705136, 51.76873716947361714, 13.79999999999999893 ) ) ;
#15586 = VERTEX_POINT ( 'NONE', #20789 ) ;
#15587 = DIRECTION ( 'NONE',  ( 0.000000000000000000, -1.000000000000000000, 0.000000000000000000 ) ) ;
#15588 = DIRECTION ( 'NONE',  ( 0.000000000000000000, 0.000000000000000000, 1.000000000000000000 ) ) ;
#15589 = DIRECTION ( 'NONE',  ( -0.000000000000000000, -0.000000000000000000, 1.000000000000000000 ) ) ;
#15590 = CIRCLE ( 'NONE', #3104, 0.04999999999999991257 ) ;
#15591 = EDGE_CURVE ( 'NONE', #18368, #20113, #21226, .T. ) ;
#15592 = ORIENTED_EDGE ( 'NONE', *, *, #853, .T. ) ;
#15593 = CIRCLE ( 'NONE', #20963, 0.5000000000000004441 ) ;
#15594 = AXIS2_PLACEMENT_3D ( 'NONE', #11010, #2507, #19408 ) ;
#15595 = ORIENTED_EDGE ( 'NONE', *, *, #16006, .T. ) ;
#15596 = ORIENTED_EDGE ( 'NONE', *, *, #20815, .T. ) ;
#15598 = B_SPLINE_CURVE_WITH_KNOTS ( 'NONE', 3,
 ( #811, #17820, #2499, #9327, #16133, #11214, #7654, #14448 ),
 .UNSPECIFIED., .F., .F.,
 ( 4, 2, 2, 4 ),
 ( -3.470042892451968281E-06, 0.0002769752510348927397, 0.0004171978979985645165, 0.0005574205449622362391 ),
 .UNSPECIFIED. ) ;
#15597 = FACE_OUTER_BOUND ( 'NONE', #2312, .T. ) ;
#15599 = CARTESIAN_POINT ( 'NONE',  ( 1.724728116533979838, 43.31054587065082728, 33.66679706732590915 ) ) ;
#15600 = CARTESIAN_POINT ( 'NONE',  ( 29.37540678000427619, 5.299999999999999822, 7.500000000000000000 ) ) ;
#15601 = FACE_OUTER_BOUND ( 'NONE', #21807, .T. ) ;
#15602 = VECTOR ( 'NONE', #11629, 1000.000000000000000 ) ;
#15603 = EDGE_CURVE ( 'NONE', #8454, #18731, #20893, .T. ) ;
#15604 = ADVANCED_FACE ( 'NONE', ( #14271 ), #17527, .T. ) ;
#15605 = EDGE_LOOP ( 'NONE', ( #5554, #16771, #8971, #21387 ) ) ;
#15606 = DIRECTION ( 'NONE',  ( 0.000000000000000000, 0.000000000000000000, -1.000000000000000000 ) ) ;
#15607 = ORIENTED_EDGE ( 'NONE', *, *, #6269, .F. ) ;
#15608 = CIRCLE ( 'NONE', #21357, 0.6000000000000033085 ) ;
#15609 = DIRECTION ( 'NONE',  ( 1.000000000000000000, 0.000000000000000000, 0.000000000000000000 ) ) ;
#15610 = CIRCLE ( 'NONE', #19555, 0.3000000000000016542 ) ;
#15611 = DIRECTION ( 'NONE',  ( 1.000000000000000000, 0.000000000000000000, 0.000000000000000000 ) ) ;
#15612 = DIRECTION ( 'NONE',  ( -0.000000000000000000, -1.000000000000000000, -0.000000000000000000 ) ) ;
#15613 = EDGE_LOOP ( 'NONE', ( #14205, #8879 ) ) ;
#15614 = FACE_OUTER_BOUND ( 'NONE', #13806, .T. ) ;
#15615 = TOROIDAL_SURFACE ( 'NONE', #3130, 0.05000000000000000278, 0.05000000000000000278 ) ;
#15616 = DIRECTION ( 'NONE',  ( -1.000000000000000000, 0.000000000000000000, 0.000000000000000000 ) ) ;
#15617 = DIRECTION ( 'NONE',  ( 0.000000000000000000, 0.000000000000000000, 1.000000000000000000 ) ) ;
#15618 = ORIENTED_EDGE ( 'NONE', *, *, #19273, .F. ) ;
#15619 = DIRECTION ( 'NONE',  ( 0.000000000000000000, 1.000000000000000000, 0.000000000000000000 ) ) ;
#15620 = VECTOR ( 'NONE', #18171, 1000.000000000000000 ) ;
#15621 = AXIS2_PLACEMENT_3D ( 'NONE', #1020, #21852, #6533 ) ;
#15622 = EDGE_CURVE ( 'NONE', #11436, #2085, #3791, .T. ) ;
#15623 = ORIENTED_EDGE ( 'NONE', *, *, #2148, .F. ) ;
#15624 = DIRECTION ( 'NONE',  ( -1.000000000000000000, 0.000000000000000000, -0.000000000000000000 ) ) ;
#15625 = ORIENTED_EDGE ( 'NONE', *, *, #7618, .T. ) ;
#15626 = VERTEX_POINT ( 'NONE', #2196 ) ;
#15627 = CARTESIAN_POINT ( 'NONE',  ( 1.724728116533979616, 43.26054587065083012, 51.80876104995653719 ) ) ;
#15628 = CIRCLE ( 'NONE', #21728, 0.1000000000000028644 ) ;
#15629 = VECTOR ( 'NONE', #3795, 1000.000000000000000 ) ;
#15630 = CIRCLE ( 'NONE', #11710, 0.2999999999999999889 ) ;
#15631 = VERTEX_POINT ( 'NONE', #9030 ) ;
#15632 = EDGE_CURVE ( 'NONE', #7129, #9421, #5797, .T. ) ;
#15633 = ADVANCED_FACE ( 'NONE', ( #4095 ), #2524, .T. ) ;
#15634 = ADVANCED_FACE ( 'NONE', ( #9248 ), #16049, .F. ) ;
#15635 = TOROIDAL_SURFACE ( 'NONE', #9584, 0.2999999999999999889, 0.2999999999999999889 ) ;
#15636 = VERTEX_POINT ( 'NONE', #16260 ) ;
#15637 = VECTOR ( 'NONE', #5421, 1000.000000000000000 ) ;
#15638 = CIRCLE ( 'NONE', #11367, 0.5000000000000004441 ) ;
#15639 = ORIENTED_EDGE ( 'NONE', *, *, #2520, .F. ) ;
#15640 = DIRECTION ( 'NONE',  ( -0.000000000000000000, -0.000000000000000000, -1.000000000000000000 ) ) ;
#15641 = CARTESIAN_POINT ( 'NONE',  ( 27.67540678000427690, 10.94079601157914539, 13.79999999999999893 ) ) ;
#15642 = FACE_OUTER_BOUND ( 'NONE', #7911, .T. ) ;
#15643 = DIRECTION ( 'NONE',  ( 0.000000000000000000, 0.000000000000000000, 1.000000000000000000 ) ) ;
#15644 = LINE ( 'NONE', #649, #3633 ) ;
#15645 = UNCERTAINTY_MEASURE_WITH_UNIT (LENGTH_MEASURE( 1.000000000000000082E-05 ), #12874, 'distance_accuracy_value', 'NONE');
#15646 = ORIENTED_EDGE ( 'NONE', *, *, #20302, .T. ) ;
#15647 = CIRCLE ( 'NONE', #2786, 0.09999999999999939493 ) ;
#15648 = AXIS2_PLACEMENT_3D ( 'NONE', #21924, #6495, #11598 ) ;
#15649 = DIRECTION ( 'NONE',  ( 0.000000000000000000, 0.000000000000000000, 1.000000000000000000 ) ) ;
#15650 = ADVANCED_FACE ( 'NONE', ( #2865 ), #11463, .T. ) ;
#15651 = DIRECTION ( 'NONE',  ( -0.000000000000000000, 0.000000000000000000, 1.000000000000000000 ) ) ;
#15652 = CIRCLE ( 'NONE', #6036, 1.500000000000001332 ) ;
#15653 = DIRECTION ( 'NONE',  ( 0.000000000000000000, 0.000000000000000000, 1.000000000000000000 ) ) ;
#15654 = AXIS2_PLACEMENT_3D ( 'NONE', #10423, #3483, #4945 ) ;
#15655 = ORIENTED_EDGE ( 'NONE', *, *, #8950, .T. ) ;
#15656 = DIRECTION ( 'NONE',  ( -0.000000000000000000, 0.000000000000000000, 1.000000000000000000 ) ) ;
#15657 = CARTESIAN_POINT ( 'NONE',  ( -15.00548668436308830, 51.86811046850819906, 13.49999999999993072 ) ) ;
#15658 = VERTEX_POINT ( 'NONE', #4764 ) ;
#15659 = ORIENTED_EDGE ( 'NONE', *, *, #11188, .T. ) ;
#15660 = CARTESIAN_POINT ( 'NONE',  ( 29.13662752439705272, 0.000000000000000000, 7.200000000000000178 ) ) ;
#15661 = DIRECTION ( 'NONE',  ( 0.9219482411244461773, -0.3873131042032275095, 0.000000000000000000 ) ) ;
#15662 = EDGE_CURVE ( 'NONE', #20783, #19588, #18785, .T. ) ;
#15663 = VERTEX_POINT ( 'NONE', #21454 ) ;
#15664 = EDGE_CURVE ( 'NONE', #4617, #21291, #19650, .T. ) ;
#15665 = AXIS2_PLACEMENT_3D ( 'NONE', #1644, #22157, #5026 ) ;
#15666 = ADVANCED_FACE ( 'NONE', ( #19761 ), #4655, .F. ) ;
#15667 = DIRECTION ( 'NONE',  ( -0.000000000000000000, -1.000000000000000000, -0.000000000000000000 ) ) ;
#15668 = EDGE_LOOP ( 'NONE', ( #2510, #12401, #5254, #10116 ) ) ;
#15669 = VECTOR ( 'NONE', #2812, 1000.000000000000000 ) ;
#15670 = VERTEX_POINT ( 'NONE', #3073 ) ;
#15671 = AXIS2_PLACEMENT_3D ( 'NONE', #17776, #11171, #14516 ) ;
#15672 = CARTESIAN_POINT ( 'NONE',  ( -1.774728116533986766, 42.36054587065083155, 29.66679706732590560 ) ) ;
#15673 = CARTESIAN_POINT ( 'NONE',  ( 1.724728116533979616, 42.31054587065082728, 51.80876104995653719 ) ) ;
#15674 = CARTESIAN_POINT ( 'NONE',  ( -31.50000000000002132, 71.00000000000001421, 3.500000000000000000 ) ) ;
#15675 = DIRECTION ( 'NONE',  ( -1.734723475976806848E-16, 0.000000000000000000, 1.000000000000000000 ) ) ;
#15676 = ADVANCED_FACE ( 'NONE', ( #8124 ), #22020, .F. ) ;
#15677 = CARTESIAN_POINT ( 'NONE',  ( -23.10703542945396194, 2.595685412882489107, 13.38944394804412852 ) ) ;
#15678 = DIRECTION ( 'NONE',  ( 0.000000000000000000, 0.000000000000000000, -1.000000000000000000 ) ) ;
#15679 = CARTESIAN_POINT ( 'NONE',  ( 23.06007706085599906, -2.355179835980778513, 13.30024289742314814 ) ) ;
#15680 = DIRECTION ( 'NONE',  ( 0.000000000000000000, 0.000000000000000000, -1.000000000000000000 ) ) ;
#15681 = ADVANCED_FACE ( 'NONE', ( #16595 ), #16498, .F. ) ;
#15682 = CARTESIAN_POINT ( 'NONE',  ( -15.21174975910705207, -52.10286008774954780, 13.87500000000000000 ) ) ;
#15683 = CIRCLE ( 'NONE', #21803, 2.500000000000002220 ) ;
#15684 = VERTEX_POINT ( 'NONE', #832 ) ;
#15685 = ORIENTED_EDGE ( 'NONE', *, *, #17274, .F. ) ;
#15686 = LINE ( 'NONE', #5645, #15637 ) ;
#15687 = VECTOR ( 'NONE', #9392, 1000.000000000000000 ) ;
#15688 = FACE_OUTER_BOUND ( 'NONE', #7543, .T. ) ;
#15689 = EDGE_LOOP ( 'NONE', ( #12133, #20618, #16539, #9023 ) ) ;
#15690 = ORIENTED_EDGE ( 'NONE', *, *, #19273, .T. ) ;
#15691 = EDGE_CURVE ( 'NONE', #5083, #10170, #20222, .T. ) ;
#15692 = AXIS2_PLACEMENT_3D ( 'NONE', #15700, #17170, #5336 ) ;
#15693 = DIRECTION ( 'NONE',  ( -2.105859220307292343E-16, 1.000000000000000000, -0.000000000000000000 ) ) ;
#15694 = AXIS2_PLACEMENT_3D ( 'NONE', #12340, #2286, #19087 ) ;
#15695 = DIRECTION ( 'NONE',  ( 0.000000000000000000, 1.000000000000000000, -0.000000000000000000 ) ) ;
#15696 = ORIENTED_EDGE ( 'NONE', *, *, #12419, .F. ) ;
#15697 = DIRECTION ( 'NONE',  ( 0.000000000000000000, 0.000000000000000000, -1.000000000000000000 ) ) ;
#15698 = DIRECTION ( 'NONE',  ( 0.000000000000000000, 0.000000000000000000, -1.000000000000000000 ) ) ;
#15699 = CARTESIAN_POINT ( 'NONE',  ( 29.37540678000427619, 6.000000000000000000, 3.799999999999999822 ) ) ;
#15700 = CARTESIAN_POINT ( 'NONE',  ( 0.000000000000000000, -52.11873716947361856, 109.6002446535588319 ) ) ;
#15701 = DIRECTION ( 'NONE',  ( 0.000000000000000000, 0.000000000000000000, 1.000000000000000000 ) ) ;
#15702 = CARTESIAN_POINT ( 'NONE',  ( -14.96174975910705207, 41.81054587065082728, 13.75000000000000000 ) ) ;
#15703 = EDGE_CURVE ( 'NONE', #13377, #3489, #11277, .T. ) ;
#15704 = ORIENTED_EDGE ( 'NONE', *, *, #1999, .T. ) ;
#15705 = LINE ( 'NONE', #19508, #7930 ) ;
#15706 = DIRECTION ( 'NONE',  ( 0.000000000000000000, 0.000000000000000000, -1.000000000000000000 ) ) ;
#15707 = EDGE_CURVE ( 'NONE', #1398, #17156, #21565, .T. ) ;
#15708 = CARTESIAN_POINT ( 'NONE',  ( -1.824728116533986810, 43.31054587065082728, 27.80876104995653719 ) ) ;
#15709 = EDGE_CURVE ( 'NONE', #19513, #2319, #19870, .T. ) ;
#15710 = EDGE_LOOP ( 'NONE', ( #13306, #2723, #11114, #13439 ) ) ;
#15711 = ORIENTED_EDGE ( 'NONE', *, *, #5605, .F. ) ;
#15712 = ORIENTED_EDGE ( 'NONE', *, *, #518, .T. ) ;
#15713 = LINE ( 'NONE', #12237, #7787 ) ;
#15714 = FACE_OUTER_BOUND ( 'NONE', #12511, .T. ) ;
#15715 =( REPRESENTATION_RELATIONSHIP ('NONE','NONE', #561, #7461 ) REPRESENTATION_RELATIONSHIP_WITH_TRANSFORMATION ( #19364 )SHAPE_REPRESENTATION_RELATIONSHIP( ) );
#15716 = TOROIDAL_SURFACE ( 'NONE', #17512, 1.300000000000000044, 0.2999999999999999889 ) ;
#15717 = SPHERICAL_SURFACE ( 'NONE', #3938, 0.5000000000000000000 ) ;
#15718 = VECTOR ( 'NONE', #10590, 1000.000000000000000 ) ;
#15719 = STYLED_ITEM ( 'NONE', ( #16693 ), #20415 ) ;
#15720 = DIRECTION ( 'NONE',  ( 2.107255972849994642E-16, -0.000000000000000000, 1.000000000000000000 ) ) ;
#15721 = EDGE_LOOP ( 'NONE', ( #20550, #10839, #6247, #19721 ) ) ;
#15722 = CYLINDRICAL_SURFACE ( 'NONE', #10068, 0.5000000000000004441 ) ;
#15723 = ORIENTED_EDGE ( 'NONE', *, *, #16684, .T. ) ;
#15724 = FACE_OUTER_BOUND ( 'NONE', #7682, .T. ) ;
#15725 = CARTESIAN_POINT ( 'NONE',  ( 9.178906393579156386, 42.46645089659917716, 68.50000000000000000 ) ) ;
#15726 = EDGE_CURVE ( 'NONE', #17432, #13921, #3434, .T. ) ;
#15727 = LINE ( 'NONE', #3892, #7233 ) ;
#15728 = ORIENTED_EDGE ( 'NONE', *, *, #19930, .T. ) ;
#15729 = CARTESIAN_POINT ( 'NONE',  ( -1.724728116533986721, 43.31054587065082728, 33.66679706732590915 ) ) ;
#15730 = DIRECTION ( 'NONE',  ( 0.000000000000000000, 0.000000000000000000, -1.000000000000000000 ) ) ;
#15731 = AXIS2_PLACEMENT_3D ( 'NONE', #5326, #12735, #19589 ) ;
#15732 = AXIS2_PLACEMENT_3D ( 'NONE', #7092, #20946, #14218 ) ;
#15733 = DIRECTION ( 'NONE',  ( -1.224646799147353207E-16, -0.000000000000000000, -1.000000000000000000 ) ) ;
#15734 = PLANE ( 'NONE',  #17463 ) ;
#15735 = ORIENTED_EDGE ( 'NONE', *, *, #10049, .F. ) ;
#15736 = ADVANCED_FACE ( 'NONE', ( #17957 ), #7798, .F. ) ;
#15737 = ORIENTED_EDGE ( 'NONE', *, *, #13236, .F. ) ;
#15738 = CARTESIAN_POINT ( 'NONE',  ( -1.724728116533986721, 43.31054587065082728, 45.66679706732590205 ) ) ;
#15739 = FACE_OUTER_BOUND ( 'NONE', #7550, .T. ) ;
#15740 = ORIENTED_EDGE ( 'NONE', *, *, #2943, .T. ) ;
#15741 = ORIENTED_EDGE ( 'NONE', *, *, #17869, .F. ) ;
#15742 = CARTESIAN_POINT ( 'NONE',  ( 31.50000000000002132, -71.00000000000001421, 3.500000000000000000 ) ) ;
#15743 = FACE_OUTER_BOUND ( 'NONE', #7027, .T. ) ;
#15744 = ORIENTED_EDGE ( 'NONE', *, *, #10795, .F. ) ;
#15745 = ORIENTED_EDGE ( 'NONE', *, *, #15767, .T. ) ;
#15746 = TOROIDAL_SURFACE ( 'NONE', #9699, 0.05000000000000000278, 0.05000000000000000278 ) ;
#15747 = ORIENTED_EDGE ( 'NONE', *, *, #10098, .F. ) ;
#15748 = ORIENTED_EDGE ( 'NONE', *, *, #10244, .T. ) ;
#15749 = DIRECTION ( 'NONE',  ( 0.000000000000000000, 0.000000000000000000, 1.000000000000000000 ) ) ;
#15750 = CYLINDRICAL_SURFACE ( 'NONE', #4368, 2.000000000000001776 ) ;
#15751 = CARTESIAN_POINT ( 'NONE',  ( 3.627054932750481964, -32.93424481021354921, 42.50000000000000000 ) ) ;
#15752 = AXIS2_PLACEMENT_3D ( 'NONE', #5337, #20540, #18975 ) ;
#15753 = VECTOR ( 'NONE', #9680, 1000.000000000000000 ) ;
#15754 = FACE_OUTER_BOUND ( 'NONE', #15470, .T. ) ;
#15755 = VERTEX_POINT ( 'NONE', #18294 ) ;
#15756 = CARTESIAN_POINT ( 'NONE',  ( 14.90249074642385096, 52.32070855895314310, 13.50000000000000178 ) ) ;
#15757 = EDGE_CURVE ( 'NONE', #13328, #1975, #6014, .T. ) ;
#15758 = CIRCLE ( 'NONE', #11073, 0.04999999999999991257 ) ;
#15759 = CARTESIAN_POINT ( 'NONE',  ( -1.724728116533986721, 43.31054587065082728, 29.66679706732590560 ) ) ;
#15760 = EDGE_CURVE ( 'NONE', #7335, #13226, #15548, .T. ) ;
#15761 = CARTESIAN_POINT ( 'NONE',  ( 29.13662752439705272, 0.000000000000000000, 7.500000000000000000 ) ) ;
#15762 = EDGE_LOOP ( 'NONE', ( #20452, #7542, #15820, #19305 ) ) ;
#15763 = DIRECTION ( 'NONE',  ( 1.000000000000000000, 0.000000000000000000, 0.000000000000000000 ) ) ;
#15764 = ORIENTED_EDGE ( 'NONE', *, *, #8500, .T. ) ;
#15765 = CIRCLE ( 'NONE', #4702, 0.2999999999999999334 ) ;
#15766 = ORIENTED_EDGE ( 'NONE', *, *, #15828, .T. ) ;
#15767 = EDGE_CURVE ( 'NONE', #17212, #10568, #18817, .T. ) ;
#15768 = APPLICATION_PROTOCOL_DEFINITION ( 'draft international standard', 'automotive_design', 1998, #6897 ) ;
#15769 = ORIENTED_EDGE ( 'NONE', *, *, #2107, .F. ) ;
#15770 = AXIS2_PLACEMENT_3D ( 'NONE', #15527, #3353, #201 ) ;
#15771 = ORIENTED_EDGE ( 'NONE', *, *, #22021, .T. ) ;
#15772 = ADVANCED_FACE ( 'NONE', ( #19869 ), #15146, .F. ) ;
#15773 = DIRECTION ( 'NONE',  ( 0.000000000000000000, 0.000000000000000000, 1.000000000000000000 ) ) ;
#15774 = EDGE_LOOP ( 'NONE', ( #5624, #3098, #7460, #2601 ) ) ;
#15775 = VERTEX_POINT ( 'NONE', #8446 ) ;
#15776 = FACE_OUTER_BOUND ( 'NONE', #3664, .T. ) ;
#15777 = LINE ( 'NONE', #15551, #15217 ) ;
#15778 = CARTESIAN_POINT ( 'NONE',  ( -34.40000000000001279, 84.70000000000001705, 79.39999999999999147 ) ) ;
#15779 = FACE_OUTER_BOUND ( 'NONE', #13776, .T. ) ;
#15780 = EDGE_CURVE ( 'NONE', #14823, #398, #13589, .T. ) ;
#15781 = VECTOR ( 'NONE', #11624, 1000.000000000000000 ) ;
#15782 = EDGE_CURVE ( 'NONE', #9791, #16858, #3453, .T. ) ;
#15783 = CARTESIAN_POINT ( 'NONE',  ( -24.69594744299175915, 42.46645089659918426, 68.25000000000000000 ) ) ;
#15784 = CIRCLE ( 'NONE', #19382, 0.2999999999999999334 ) ;
#15785 = ADVANCED_FACE ( 'NONE', ( #15262 ), #3192, .F. ) ;
#15786 = DIRECTION ( 'NONE',  ( 0.000000000000000000, 0.000000000000000000, -1.000000000000000000 ) ) ;
#15787 = DIRECTION ( 'NONE',  ( 1.000000000000000000, 0.000000000000000000, 0.000000000000000000 ) ) ;
#15788 = DIRECTION ( 'NONE',  ( 1.000000000000000000, 0.000000000000000000, 0.000000000000000000 ) ) ;
#15789 = EDGE_CURVE ( 'NONE', #5745, #21866, #10238, .T. ) ;
#15790 = CARTESIAN_POINT ( 'NONE',  ( -1.824728116533986810, 42.36054587065083155, 43.70876104995653577 ) ) ;
#15791 = ORIENTED_EDGE ( 'NONE', *, *, #1124, .T. ) ;
#15792 = ORIENTED_EDGE ( 'NONE', *, *, #5946, .F. ) ;
#15793 = DIRECTION ( 'NONE',  ( 0.000000000000000000, -1.000000000000000000, 0.000000000000000000 ) ) ;
#15794 = LINE ( 'NONE', #12112, #17764 ) ;
#15795 = ORIENTED_EDGE ( 'NONE', *, *, #7285, .T. ) ;
#15796 = ORIENTED_EDGE ( 'NONE', *, *, #1937, .T. ) ;
#15797 = CIRCLE ( 'NONE', #18673, 0.04999999999999991257 ) ;
#15798 = EDGE_CURVE ( 'NONE', #17367, #16560, #20194, .T. ) ;
#15799 = CIRCLE ( 'NONE', #4338, 0.2999999999999999334 ) ;
#15800 = DIRECTION ( 'NONE',  ( -1.000000000000000000, 0.000000000000000000, 0.000000000000000000 ) ) ;
#15801 = CARTESIAN_POINT ( 'NONE',  ( 23.04273156199908357, 2.261510999192739124, 7.500000000000000000 ) ) ;
#15802 = ORIENTED_EDGE ( 'NONE', *, *, #2170, .F. ) ;
#15803 = CARTESIAN_POINT ( 'NONE',  ( -23.04273156199908357, 2.261510999192739124, 7.500000000000000000 ) ) ;
#15804 = AXIS2_PLACEMENT_3D ( 'NONE', #17905, #12862, #10977 ) ;
#15805 = PLANE ( 'NONE',  #310 ) ;
#15806 = CARTESIAN_POINT ( 'NONE',  ( -29.50000000000002132, -2.473451120191013430, 1.500000000000001332 ) ) ;
#15807 = ADVANCED_FACE ( 'NONE', ( #151 ), #4985, .T. ) ;
#15808 = CARTESIAN_POINT ( 'NONE',  ( -1.724728116533986721, 43.26054587065083012, 39.80876104995653719 ) ) ;
#15809 = DIRECTION ( 'NONE',  ( 0.000000000000000000, 1.000000000000000000, 0.000000000000000000 ) ) ;
#15810 = DIRECTION ( 'NONE',  ( 0.000000000000000000, 0.000000000000000000, 1.000000000000000000 ) ) ;
#15811 = EDGE_CURVE ( 'NONE', #20727, #19232, #13775, .T. ) ;
#15812 = ORIENTED_EDGE ( 'NONE', *, *, #18196, .T. ) ;
#15813 = DIRECTION ( 'NONE',  ( -1.000000000000000000, 0.000000000000000000, 0.000000000000000000 ) ) ;
#15814 = DIRECTION ( 'NONE',  ( 0.000000000000000000, 0.000000000000000000, 1.000000000000000000 ) ) ;
#15815 = DIRECTION ( 'NONE',  ( -0.000000000000000000, -1.000000000000000000, -0.000000000000000000 ) ) ;
#15816 = EDGE_LOOP ( 'NONE', ( #5564, #12921, #10320, #927 ) ) ;
#15817 = ORIENTED_EDGE ( 'NONE', *, *, #12218, .T. ) ;
#15818 = CARTESIAN_POINT ( 'NONE',  ( -21.92816239687475743, 42.46645089659918426, 68.25000000000000000 ) ) ;
#15819 = DIRECTION ( 'NONE',  ( 1.000000000000000000, -0.000000000000000000, 0.000000000000000000 ) ) ;
#15820 = ORIENTED_EDGE ( 'NONE', *, *, #10242, .T. ) ;
#15821 = CARTESIAN_POINT ( 'NONE',  ( 15.21174975910705918, 41.81054587065082728, 13.75000000000000000 ) ) ;
#15822 = EDGE_LOOP ( 'NONE', ( #6085, #5374, #6145, #6063 ) ) ;
#15823 = DIRECTION ( 'NONE',  ( -1.000000000000000000, 0.000000000000000000, 0.000000000000000000 ) ) ;
#15824 = DIRECTION ( 'NONE',  ( -1.000000000000000000, 0.000000000000000000, 0.000000000000000000 ) ) ;
#15825 = ADVANCED_FACE ( 'NONE', ( #6999 ), #13473, .T. ) ;
#15826 = VERTEX_POINT ( 'NONE', #6791 ) ;
#15827 = CARTESIAN_POINT ( 'NONE',  ( -28.82574430125643516, -6.542305536751587880, 13.37088755551135932 ) ) ;
#15828 = EDGE_CURVE ( 'NONE', #1525, #2296, #2718, .T. ) ;
#15829 = CARTESIAN_POINT ( 'NONE',  ( 1.724728116533979838, 42.36054587065083155, 29.66679706732590560 ) ) ;
#15830 = CARTESIAN_POINT ( 'NONE',  ( -25.37540678000429395, -39.04634676501046187, 13.50000000000000000 ) ) ;
#15831 = ORIENTED_EDGE ( 'NONE', *, *, #8938, .T. ) ;
#15832 = LINE ( 'NONE', #19323, #20950 ) ;
#15833 = DIRECTION ( 'NONE',  ( 1.000000000000000000, 0.000000000000000000, 0.000000000000000000 ) ) ;
#15834 = CARTESIAN_POINT ( 'NONE',  ( -30.49999999999999289, -85.00000000000000000, 1.199999999999999734 ) ) ;
#15835 = CARTESIAN_POINT ( 'NONE',  ( -31.26086011588028057, 83.95073979834609190, 13.75000000000000000 ) ) ;
#15836 = ORIENTED_EDGE ( 'NONE', *, *, #8072, .F. ) ;
#15837 = DIRECTION ( 'NONE',  ( 2.107255972849994642E-16, -0.000000000000000000, 1.000000000000000000 ) ) ;
#15838 = ADVANCED_FACE ( 'NONE', ( #1502 ), #3074, .T. ) ;
#15839 = ORIENTED_EDGE ( 'NONE', *, *, #19898, .T. ) ;
#15840 = CARTESIAN_POINT ( 'NONE',  ( 15.95292532278785913, 34.11873716947361856, 42.50000000000000711 ) ) ;
#15841 = LINE ( 'NONE', #5479, #8462 ) ;
#15842 =( GEOMETRIC_REPRESENTATION_CONTEXT ( 3 ) GLOBAL_UNCERTAINTY_ASSIGNED_CONTEXT ( ( #7171 ) ) GLOBAL_UNIT_ASSIGNED_CONTEXT ( ( #245, #14006, #20636 ) ) REPRESENTATION_CONTEXT ( 'NONE', 'WORKASPACE' ) );
#15843 = ORIENTED_EDGE ( 'NONE', *, *, #4671, .F. ) ;
#15844 = VERTEX_POINT ( 'NONE', #20535 ) ;
#15845 = DIRECTION ( 'NONE',  ( 0.000000000000000000, 1.000000000000000000, 0.000000000000000000 ) ) ;
#15846 = DIRECTION ( 'NONE',  ( -1.000000000000000000, 0.000000000000000000, 0.000000000000000000 ) ) ;
#15847 = VERTEX_POINT ( 'NONE', #5096 ) ;
#15848 = AXIS2_PLACEMENT_3D ( 'NONE', #9035, #17414, #19003 ) ;
#15849 = ORIENTED_EDGE ( 'NONE', *, *, #2502, .F. ) ;
#15850 = EDGE_CURVE ( 'NONE', #10573, #5066, #12004, .T. ) ;
#15851 = ORIENTED_EDGE ( 'NONE', *, *, #9967, .T. ) ;
#15852 = CARTESIAN_POINT ( 'NONE',  ( -1.724728116533986721, 42.31054587065082728, 33.71679706732589921 ) ) ;
#15853 = AXIS2_PLACEMENT_3D ( 'NONE', #15332, #10310, #8193 ) ;
#15854 = EDGE_CURVE ( 'NONE', #22008, #20718, #1390, .T. ) ;
#15855 = AXIS2_PLACEMENT_3D ( 'NONE', #15153, #17059, #14936 ) ;
#15856 = DIRECTION ( 'NONE',  ( 0.000000000000000000, -1.000000000000000000, 0.000000000000000000 ) ) ;
#15857 = DIRECTION ( 'NONE',  ( 0.000000000000000000, 0.000000000000000000, -1.000000000000000000 ) ) ;
#15858 = EDGE_LOOP ( 'NONE', ( #19286, #6103, #6658, #4584 ) ) ;
#15859 = LINE ( 'NONE', #19353, #9637 ) ;
#15860 = DIRECTION ( 'NONE',  ( -0.000000000000000000, -1.000000000000000000, -0.000000000000000000 ) ) ;
#15861 = CARTESIAN_POINT ( 'NONE',  ( 1.824728116533979261, 43.31054587065082728, 35.80876104995653009 ) ) ;
#15862 = VERTEX_POINT ( 'NONE', #12118 ) ;
#15863 = CARTESIAN_POINT ( 'NONE',  ( 18.22752199202934520, 39.04634676501046187, 13.50000000000000000 ) ) ;
#15864 = ORIENTED_EDGE ( 'NONE', *, *, #17119, .T. ) ;
#15865 = EDGE_CURVE ( 'NONE', #10431, #17181, #18735, .T. ) ;
#15866 = ORIENTED_EDGE ( 'NONE', *, *, #15304, .T. ) ;
#15867 = VECTOR ( 'NONE', #13086, 1000.000000000000000 ) ;
#15868 = EDGE_LOOP ( 'NONE', ( #4627, #11249, #2985, #17816 ) ) ;
#15869 = DIRECTION ( 'NONE',  ( 0.000000000000000000, -1.000000000000000000, 0.000000000000000000 ) ) ;
#15870 = ITEM_DEFINED_TRANSFORMATION ( 'NONE', 'NONE', #18357,  #17493 ) ;
#15871 = VERTEX_POINT ( 'NONE', #13686 ) ;
#15872 = ORIENTED_EDGE ( 'NONE', *, *, #7666, .F. ) ;
#15873 = EDGE_CURVE ( 'NONE', #12188, #13276, #6319, .T. ) ;
#15874 = DIRECTION ( 'NONE',  ( -0.000000000000000000, -1.000000000000000000, -0.000000000000000000 ) ) ;
#15875 = EDGE_LOOP ( 'NONE', ( #3049, #14670, #9570, #5340 ) ) ;
#15876 = ORIENTED_EDGE ( 'NONE', *, *, #15865, .F. ) ;
#15877 = DIRECTION ( 'NONE',  ( -1.000000000000000000, -0.000000000000000000, 0.000000000000000000 ) ) ;
#15878 = FACE_OUTER_BOUND ( 'NONE', #7128, .T. ) ;
#15879 = DIRECTION ( 'NONE',  ( 1.000000000000000000, 0.000000000000000000, 0.000000000000000000 ) ) ;
#15880 = CYLINDRICAL_SURFACE ( 'NONE', #17356, 0.3000000000000016542 ) ;
#15881 = CIRCLE ( 'NONE', #3752, 0.2999999999999999334 ) ;
#15882 = VECTOR ( 'NONE', #13398, 1000.000000000000000 ) ;
#15883 = CARTESIAN_POINT ( 'NONE',  ( -8.638906393579159015, 41.66638367286108746, 68.06527860057354928 ) ) ;
#15884 = CARTESIAN_POINT ( 'NONE',  ( 28.87540678000428329, 6.494748934539265051, 13.24746166461178554 ) ) ;
#15885 = LINE ( 'NONE', #5521, #15431 ) ;
#15886 = CARTESIAN_POINT ( 'NONE',  ( 3.127054932750481964, -32.61873716947361856, 68.00000000000000000 ) ) ;
#15887 = DIRECTION ( 'NONE',  ( -1.000000000000000000, 0.000000000000000000, -0.000000000000000000 ) ) ;
#15888 = EDGE_CURVE ( 'NONE', #17660, #10999, #17015, .T. ) ;
#15889 = VERTEX_POINT ( 'NONE', #21891 ) ;
#15890 = AXIS2_PLACEMENT_3D ( 'NONE', #3005, #11270, #8048 ) ;
#15891 = ORIENTED_EDGE ( 'NONE', *, *, #143, .F. ) ;
#15892 = DIRECTION ( 'NONE',  ( -0.000000000000000000, 0.000000000000000000, 1.000000000000000000 ) ) ;
#15893 = PRESENTATION_STYLE_ASSIGNMENT (( #16120 ) ) ;
#15894 = FACE_OUTER_BOUND ( 'NONE', #21892, .T. ) ;
#15895 = ORIENTED_EDGE ( 'NONE', *, *, #7972, .T. ) ;
#15896 = VECTOR ( 'NONE', #15391, 1000.000000000000000 ) ;
#15897 = AXIS2_PLACEMENT_3D ( 'NONE', #16369, #21543, #9677 ) ;
#15898 = EDGE_LOOP ( 'NONE', ( #10070, #2584, #9100, #18697 ) ) ;
#15899 = EDGE_CURVE ( 'NONE', #7824, #8633, #581, .T. ) ;
#15900 = ADVANCED_FACE ( 'NONE', ( #14349 ), #19293, .T. ) ;
#15901 = DIRECTION ( 'NONE',  ( 0.000000000000000000, 0.000000000000000000, -1.000000000000000000 ) ) ;
#15902 = DIRECTION ( 'NONE',  ( -1.000000000000000000, 0.000000000000000000, -0.000000000000000000 ) ) ;
#15903 = EDGE_LOOP ( 'NONE', ( #13651, #2129, #8319, #2976, #15211, #6691 ) ) ;
#15904 = CARTESIAN_POINT ( 'NONE',  ( 15.95292532278785913, -50.11873716947361856, 13.87499999999999822 ) ) ;
#15905 = CARTESIAN_POINT ( 'NONE',  ( -29.69597781366221412, 25.99124249474150972, 70.25000000000000000 ) ) ;
#15906 = DIRECTION ( 'NONE',  ( -0.000000000000000000, 1.000000000000000000, -0.000000000000000000 ) ) ;
#15907 = DIRECTION ( 'NONE',  ( 1.000000000000000000, 0.000000000000000000, 0.000000000000000000 ) ) ;
#15908 = CARTESIAN_POINT ( 'NONE',  ( -14.71432562863492421, 52.07267296161941061, 13.49999999999999822 ) ) ;
#15909 = LINE ( 'NONE', #5213, #18058 ) ;
#15910 = AXIS2_PLACEMENT_3D ( 'NONE', #9185, #15877, #5747 ) ;
#15911 = AXIS2_PLACEMENT_3D ( 'NONE', #15241, #10003, #20176 ) ;
#15912 = AXIS2_PLACEMENT_3D ( 'NONE', #177, #10488, #8603 ) ;
#15913 = EDGE_CURVE ( 'NONE', #2242, #13197, #16019, .T. ) ;
#15914 = DIRECTION ( 'NONE',  ( 0.000000000000000000, 1.000000000000000000, 0.000000000000000000 ) ) ;
#15915 = FACE_OUTER_BOUND ( 'NONE', #5176, .T. ) ;
#15916 = CARTESIAN_POINT ( 'NONE',  ( 0.000000000000000000, -32.11873716947361856, 109.6002446535588319 ) ) ;
#15917 = VERTEX_POINT ( 'NONE', #10787 ) ;
#15918 = ORIENTED_EDGE ( 'NONE', *, *, #21040, .T. ) ;
#15919 = EDGE_LOOP ( 'NONE', ( #18464, #1744, #21362, #6471 ) ) ;
#15920 = CARTESIAN_POINT ( 'NONE',  ( -15.95292532278785913, -52.11873716947361856, 14.00000000000000000 ) ) ;
#15921 = DIRECTION ( 'NONE',  ( 0.000000000000000000, 1.000000000000000000, 0.000000000000000000 ) ) ;
#15922 = AXIS2_PLACEMENT_3D ( 'NONE', #15729, #9250, #5697 ) ;
#15923 = AXIS2_PLACEMENT_3D ( 'NONE', #8003, #2621, #21442 ) ;
#15924 = AXIS2_PLACEMENT_3D ( 'NONE', #18455, #16892, #8293 ) ;
#15925 = EDGE_CURVE ( 'NONE', #6698, #7599, #12700, .T. ) ;
#15926 = EDGE_CURVE ( 'NONE', #5394, #12260, #5868, .T. ) ;
#15927 = VERTEX_POINT ( 'NONE', #17265 ) ;
#15928 = CARTESIAN_POINT ( 'NONE',  ( -9.141460742840918030, 32.93424481021354921, 68.00000000000000000 ) ) ;
#15929 = AXIS2_PLACEMENT_3D ( 'NONE', #1840, #16828, #3406 ) ;
#15930 = DIRECTION ( 'NONE',  ( 0.000000000000000000, -0.000000000000000000, 1.000000000000000000 ) ) ;
#15931 = EDGE_CURVE ( 'NONE', #20718, #5997, #257, .T. ) ;
#15932 = ORIENTED_EDGE ( 'NONE', *, *, #18225, .T. ) ;
#15933 = DIRECTION ( 'NONE',  ( 1.000000000000000000, 0.000000000000000000, 0.000000000000000000 ) ) ;
#15934 = DIRECTION ( 'NONE',  ( 1.000000000000000000, 0.000000000000000000, 0.000000000000000000 ) ) ;
#15935 = CARTESIAN_POINT ( 'NONE',  ( 23.02398829872514341, 2.157133568460765538, 13.26781970120005560 ) ) ;
#15936 = CARTESIAN_POINT ( 'NONE',  ( -23.32398829872514057, -2.157133568460768647, 7.500000000000000000 ) ) ;
#15937 = ORIENTED_EDGE ( 'NONE', *, *, #16855, .F. ) ;
#15938 = CARTESIAN_POINT ( 'NONE',  ( 29.17540678000427690, -63.74634676501045050, 7.500000000000000000 ) ) ;
#15939 = CARTESIAN_POINT ( 'NONE',  ( -1.774728116533986544, 42.31054587065082728, 27.80876104995653719 ) ) ;
#15940 = CARTESIAN_POINT ( 'NONE',  ( -35.00000000000001421, 84.70000000000001705, 79.39999999999999147 ) ) ;
#15941 = DIRECTION ( 'NONE',  ( -0.000000000000000000, -1.000000000000000000, -0.000000000000000000 ) ) ;
#15942 = EDGE_LOOP ( 'NONE', ( #20485, #11115, #15380, #12478 ) ) ;
#15943 = VECTOR ( 'NONE', #12576, 1000.000000000000000 ) ;
#15944 = AXIS2_PLACEMENT_3D ( 'NONE', #4766, #11465, #3076 ) ;
#15945 = AXIS2_PLACEMENT_3D ( 'NONE', #3572, #10399, #4108 ) ;
#15946 = AXIS2_PLACEMENT_3D ( 'NONE', #4476, #21395, #21181 ) ;
#15947 = ORIENTED_EDGE ( 'NONE', *, *, #9724, .F. ) ;
#15948 = CARTESIAN_POINT ( 'NONE',  ( -9.641460742840918030, 32.61873716947361856, 109.6002446535588319 ) ) ;
#15949 = DIRECTION ( 'NONE',  ( 0.000000000000000000, 0.000000000000000000, -1.000000000000000000 ) ) ;
#15950 = ORIENTED_EDGE ( 'NONE', *, *, #4895, .T. ) ;
#15951 = VERTEX_POINT ( 'NONE', #697 ) ;
#15952 = FACE_OUTER_BOUND ( 'NONE', #4303, .T. ) ;
#15953 = EDGE_CURVE ( 'NONE', #1252, #6865, #4146, .T. ) ;
#15954 = CARTESIAN_POINT ( 'NONE',  ( 14.71174975910706983, 52.11873716947361856, 68.00000000000000000 ) ) ;
#15955 = ORIENTED_EDGE ( 'NONE', *, *, #18351, .T. ) ;
#15956 = AXIS2_PLACEMENT_3D ( 'NONE', #11676, #3302, #3525 ) ;
#15957 = ORIENTED_EDGE ( 'NONE', *, *, #20856, .T. ) ;
#15958 = AXIS2_PLACEMENT_3D ( 'NONE', #13413, #20252, #18120 ) ;
#15959 = EDGE_CURVE ( 'NONE', #18447, #6635, #12444, .T. ) ;
#15960 = AXIS2_PLACEMENT_3D ( 'NONE', #16867, #1533, #8370 ) ;
#15961 = ORIENTED_EDGE ( 'NONE', *, *, #172, .F. ) ;
#15962 = CARTESIAN_POINT ( 'NONE',  ( -31.50000000000002132, 71.70000000000001705, 1.500000000000000000 ) ) ;
#15963 = CIRCLE ( 'NONE', #12386, 0.4999999999999995559 ) ;
#15964 = B_SPLINE_CURVE_WITH_KNOTS ( 'NONE', 3,
 ( #7703, #14507, #3800, #3921, #10739, #17553 ),
 .UNSPECIFIED., .F., .F.,
 ( 4, 2, 4 ),
 ( 0.000000000000000000, 0.0002343434414548649890, 0.0004686868829097299780 ),
 .UNSPECIFIED. ) ;
#15965 = AXIS2_PLACEMENT_3D ( 'NONE', #16738, #8143, #1404 ) ;
#15966 = LINE ( 'NONE', #7382, #4025 ) ;
#15967 = CARTESIAN_POINT ( 'NONE',  ( 17.45292532278785913, 50.11873716947361856, 68.00000000000000000 ) ) ;
#15968 = CARTESIAN_POINT ( 'NONE',  ( 1.724728116533979838, 43.26054587065083012, 37.66679706732590915 ) ) ;
#15969 = ORIENTED_EDGE ( 'NONE', *, *, #5862, .T. ) ;
#15970 = CARTESIAN_POINT ( 'NONE',  ( 29.50000000000002132, 2.512390033608338680, 0.2497329951907094336 ) ) ;
#15971 = FACE_OUTER_BOUND ( 'NONE', #21349, .T. ) ;
#15972 = DIRECTION ( 'NONE',  ( -0.000000000000000000, 0.000000000000000000, 1.000000000000000000 ) ) ;
#15973 = VECTOR ( 'NONE', #18320, 1000.000000000000000 ) ;
#15974 = VECTOR ( 'NONE', #13867, 1000.000000000000000 ) ;
#15975 = ORIENTED_EDGE ( 'NONE', *, *, #11193, .F. ) ;
#15976 = EDGE_CURVE ( 'NONE', #4042, #5726, #8890, .T. ) ;
#15977 = DIRECTION ( 'NONE',  ( 0.000000000000000000, -1.000000000000000000, 0.000000000000000000 ) ) ;
#15978 = ORIENTED_EDGE ( 'NONE', *, *, #4443, .F. ) ;
#15979 = AXIS2_PLACEMENT_3D ( 'NONE', #19829, #2369, #18142 ) ;
#15980 = ADVANCED_FACE ( 'NONE', ( #15577 ), #9150, .T. ) ;
#15981 = ORIENTED_EDGE ( 'NONE', *, *, #2567, .F. ) ;
#15982 = CIRCLE ( 'NONE', #13835, 0.2500000000000002220 ) ;
#15983 = VERTEX_POINT ( 'NONE', #19069 ) ;
#15984 = CARTESIAN_POINT ( 'NONE',  ( 33.49999999999999289, -85.00000000000000000, 1.799999999999996048 ) ) ;
#15985 = VECTOR ( 'NONE', #18313, 1000.000000000000000 ) ;
#15986 = VERTEX_POINT ( 'NONE', #12550 ) ;
#15987 = EDGE_LOOP ( 'NONE', ( #10286, #9740, #18741, #16307 ) ) ;
#15988 = CARTESIAN_POINT ( 'NONE',  ( 23.02398829872514341, -2.246571036181248981, 13.29719918165956294 ) ) ;
#15989 = ORIENTED_EDGE ( 'NONE', *, *, #996, .F. ) ;
#15990 = DIRECTION ( 'NONE',  ( 0.000000000000000000, -1.000000000000000000, 0.000000000000000000 ) ) ;
#15991 = AXIS2_PLACEMENT_3D ( 'NONE', #1163, #4654, #13139 ) ;
#15992 = CIRCLE ( 'NONE', #19231, 0.5000000000000004441 ) ;
#15993 = CARTESIAN_POINT ( 'NONE',  ( -29.13662752439705272, 0.000000000000000000, 1.500000000000001332 ) ) ;
#15994 = DIRECTION ( 'NONE',  ( 0.000000000000000000, -1.000000000000000000, 0.000000000000000000 ) ) ;
#15995 = CARTESIAN_POINT ( 'NONE',  ( -29.37540678000427619, -6.000000000000000000, 7.500000000000000000 ) ) ;
#15996 = AXIS2_PLACEMENT_3D ( 'NONE', #2113, #7169, #13853 ) ;
#15997 = ADVANCED_FACE ( 'NONE', ( #19395 ), #20757, .T. ) ;
#15998 = CIRCLE ( 'NONE', #6394, 2.274596669241483848 ) ;
#15999 = DIRECTION ( 'NONE',  ( 0.000000000000000000, 0.000000000000000000, -1.000000000000000000 ) ) ;
#16000 = CIRCLE ( 'NONE', #3878, 0.5000000000000004441 ) ;
#16001 =( REPRESENTATION_RELATIONSHIP ('NONE','NONE', #561, #7461 ) REPRESENTATION_RELATIONSHIP_WITH_TRANSFORMATION ( #21611 )SHAPE_REPRESENTATION_RELATIONSHIP( ) );
#16002 = CARTESIAN_POINT ( 'NONE',  ( -23.04273156199908357, 2.261510999192889670, 13.19999999999999218 ) ) ;
#16003 = DIRECTION ( 'NONE',  ( 0.000000000000000000, -0.000000000000000000, 1.000000000000000000 ) ) ;
#16004 = DIRECTION ( 'NONE',  ( 0.000000000000000000, 0.000000000000000000, 1.000000000000000000 ) ) ;
#16005 = CARTESIAN_POINT ( 'NONE',  ( 1.774728116533979660, 43.26054587065083012, 31.80876104995653719 ) ) ;
#16006 = EDGE_CURVE ( 'NONE', #4820, #6732, #5433, .T. ) ;
#16007 = EDGE_LOOP ( 'NONE', ( #12291, #13323, #16736, #8270 ) ) ;
#16008 = ORIENTED_EDGE ( 'NONE', *, *, #5530, .T. ) ;
#16009 = DIRECTION ( 'NONE',  ( -0.000000000000000000, -1.000000000000000000, 0.000000000000000000 ) ) ;
#16010 = VECTOR ( 'NONE', #15077, 1000.000000000000000 ) ;
#16011 = ORIENTED_EDGE ( 'NONE', *, *, #2550, .F. ) ;
#16012 = TOROIDAL_SURFACE ( 'NONE', #18905, 0.2500000000000000000, 0.2500000000000000000 ) ;
#16013 = ORIENTED_EDGE ( 'NONE', *, *, #17908, .F. ) ;
#16014 = VECTOR ( 'NONE', #17359, 1000.000000000000000 ) ;
#16015 = EDGE_CURVE ( 'NONE', #12543, #18168, #4066, .T. ) ;
#16016 = DIRECTION ( 'NONE',  ( 0.000000000000000000, 1.000000000000000000, 0.000000000000000000 ) ) ;
#16017 = AXIS2_PLACEMENT_3D ( 'NONE', #18628, #16941, #22121 ) ;
#16018 = AXIS2_PLACEMENT_3D ( 'NONE', #10921, #20898, #19328 ) ;
#16019 = LINE ( 'NONE', #10555, #207 ) ;
#16020 = ORIENTED_EDGE ( 'NONE', *, *, #6041, .F. ) ;
#16021 = CARTESIAN_POINT ( 'NONE',  ( 0.000000000000000000, 0.000000000000000000, 3.500000000000000000 ) ) ;
#16022 = DIRECTION ( 'NONE',  ( -0.000000000000000000, -1.000000000000000000, -0.000000000000000000 ) ) ;
#16023 = CIRCLE ( 'NONE', #21782, 0.5000000000000004441 ) ;
#16024 = CARTESIAN_POINT ( 'NONE',  ( 14.96174975910705918, 51.76873716947361004, 13.79999999999999716 ) ) ;
#16025 = FACE_OUTER_BOUND ( 'NONE', #14295, .T. ) ;
#16026 = DIRECTION ( 'NONE',  ( 1.000000000000000000, -0.000000000000000000, 0.000000000000000000 ) ) ;
#16027 = ADVANCED_FACE ( 'NONE', ( #17374 ), #2268, .F. ) ;
#16028 = ORIENTED_EDGE ( 'NONE', *, *, #19525, .F. ) ;
#16029 = LINE ( 'NONE', #17825, #10063 ) ;
#16030 = CARTESIAN_POINT ( 'NONE',  ( 0.000000000000000000, -52.10286008774954780, 13.87500000000000000 ) ) ;
#16031 = EDGE_CURVE ( 'NONE', #8820, #5552, #7219, .T. ) ;
#16032 = DIRECTION ( 'NONE',  ( 0.000000000000000000, 0.000000000000000000, 1.000000000000000000 ) ) ;
#16033 = VERTEX_POINT ( 'NONE', #2161 ) ;
#16034 = ORIENTED_EDGE ( 'NONE', *, *, #4515, .F. ) ;
#16035 = VERTEX_POINT ( 'NONE', #9001 ) ;
#16036 = CARTESIAN_POINT ( 'NONE',  ( 31.50000000000002132, 72.00000000000001421, 3.200000000000000178 ) ) ;
#16037 = CYLINDRICAL_SURFACE ( 'NONE', #10670, 0.2500000000000002220 ) ;
#16038 = VERTEX_POINT ( 'NONE', #15801 ) ;
#16039 = CARTESIAN_POINT ( 'NONE',  ( -33.20000000000001705, 85.00000000000000000, 78.20000000000000284 ) ) ;
#16040 =( GEOMETRIC_REPRESENTATION_CONTEXT ( 3 ) GLOBAL_UNCERTAINTY_ASSIGNED_CONTEXT ( ( #19830 ) ) GLOBAL_UNIT_ASSIGNED_CONTEXT ( ( #5293, #15454, #11760 ) ) REPRESENTATION_CONTEXT ( 'NONE', 'WORKASPACE' ) );
#16041 = AXIS2_PLACEMENT_3D ( 'NONE', #10084, #13311, #3356 ) ;
#16042 = ORIENTED_EDGE ( 'NONE', *, *, #21858, .T. ) ;
#16043 = DIRECTION ( 'NONE',  ( 3.543406725251269872E-15, -1.000000000000000000, -5.100473277356134011E-17 ) ) ;
#16044 = CARTESIAN_POINT ( 'NONE',  ( -1.774728116533986544, 43.26054587065083012, 27.80876104995653719 ) ) ;
#16045 = EDGE_CURVE ( 'NONE', #4942, #2394, #470, .T. ) ;
#16046 = DIRECTION ( 'NONE',  ( -0.000000000000000000, -0.000000000000000000, 1.000000000000000000 ) ) ;
#16047 = PLANE ( 'NONE',  #7813 ) ;
#16048 = LINE ( 'NONE', #4094, #10437 ) ;
#16049 = PLANE ( 'NONE',  #7714 ) ;
#16050 = ORIENTED_EDGE ( 'NONE', *, *, #640, .T. ) ;
#16051 = CARTESIAN_POINT ( 'NONE',  ( 1.724728116533979616, 43.26054587065083012, 39.75876104995653293 ) ) ;
#16052 = DIRECTION ( 'NONE',  ( 0.000000000000000000, 0.000000000000000000, 1.000000000000000000 ) ) ;
#16053 = CARTESIAN_POINT ( 'NONE',  ( -31.69597781366222122, 56.94165929845684815, 68.75000000000000000 ) ) ;
#16054 = LINE ( 'NONE', #4006, #18534 ) ;
#16055 = VERTEX_POINT ( 'NONE', #911 ) ;
#16056 = CARTESIAN_POINT ( 'NONE',  ( 14.96174975910707161, 41.81054587065082728, 68.25000000000000000 ) ) ;
#16057 = EDGE_CURVE ( 'NONE', #3754, #15018, #12988, .T. ) ;
#16058 = VERTEX_POINT ( 'NONE', #12771 ) ;
#16059 = CIRCLE ( 'NONE', #10721, 0.2999999999999999889 ) ;
#16060 = AXIS2_PLACEMENT_3D ( 'NONE', #5870, #12222, #5435 ) ;
#16061 = DIRECTION ( 'NONE',  ( 0.000000000000000000, 1.000000000000000000, -0.000000000000000000 ) ) ;
#16062 = AXIS2_PLACEMENT_3D ( 'NONE', #486, #14259, #19309 ) ;
#16063 = ADVANCED_FACE ( 'NONE', ( #807 ), #20597, .F. ) ;
#16064 = CARTESIAN_POINT ( 'NONE',  ( -23.02398829872514341, -2.157133568460766426, 13.26781970120005738 ) ) ;
#16065 = EDGE_LOOP ( 'NONE', ( #14898, #8540, #13000, #3120 ) ) ;
#16066 = VERTEX_POINT ( 'NONE', #7986 ) ;
#16067 = DIRECTION ( 'NONE',  ( -1.000000000000000000, 0.000000000000000000, 0.000000000000000000 ) ) ;
#16069 = EDGE_CURVE ( 'NONE', #5066, #11507, #22041, .T. ) ;
#16068 = CARTESIAN_POINT ( 'NONE',  ( -3.627054932750481964, 32.93424481021354921, 68.00000000000000000 ) ) ;
#16070 = LINE ( 'NONE', #5911, #9934 ) ;
#16071 = VERTEX_POINT ( 'NONE', #5978 ) ;
#16072 = B_SPLINE_CURVE_WITH_KNOTS ( 'NONE', 3,
 ( #10698, #19606, #10477, #4279 ),
 .UNSPECIFIED., .F., .F.,
 ( 4, 4 ),
 ( 0.001759598111914162421, 0.004588913574811922039 ),
 .UNSPECIFIED. ) ;
#16073 = ORIENTED_EDGE ( 'NONE', *, *, #6466, .F. ) ;
#16074 = CIRCLE ( 'NONE', #9685, 2.000000000000001776 ) ;
#16075 = ADVANCED_FACE ( 'NONE', ( #9773 ), #4503, .T. ) ;
#16076 = VERTEX_POINT ( 'NONE', #21757 ) ;
#16077 = FACE_OUTER_BOUND ( 'NONE', #13687, .T. ) ;
#16078 = CIRCLE ( 'NONE', #21831, 0.2999999999999999334 ) ;
#16079 = DIRECTION ( 'NONE',  ( 0.000000000000000000, 0.000000000000000000, -1.000000000000000000 ) ) ;
#16080 = DIRECTION ( 'NONE',  ( 1.000000000000000000, -0.000000000000000000, -0.000000000000000000 ) ) ;
#16081 = CARTESIAN_POINT ( 'NONE',  ( -1.774728116533986766, 42.31054587065082728, 41.66679706732590915 ) ) ;
#16082 = ORIENTED_EDGE ( 'NONE', *, *, #21964, .F. ) ;
#16083 = DIRECTION ( 'NONE',  ( 0.000000000000000000, 1.000000000000000000, -0.000000000000000000 ) ) ;
#16084 = CARTESIAN_POINT ( 'NONE',  ( -10.73004499984425841, -2.546852060775806059, 13.75000000000000000 ) ) ;
#16085 = ADVANCED_FACE ( 'NONE', ( #16572 ), #14790, .F. ) ;
#16086 = CARTESIAN_POINT ( 'NONE',  ( -1.724728116533986721, 43.31054587065082728, 33.71679706732589921 ) ) ;
#16088 = EDGE_CURVE ( 'NONE', #4856, #20038, #21313, .T. ) ;
#16087 = PLANE ( 'NONE',  #13172 ) ;
#16089 = VECTOR ( 'NONE', #17967, 1000.000000000000000 ) ;
#16090 = EDGE_LOOP ( 'NONE', ( #16513, #1377, #7756, #21227 ) ) ;
#16091 = DIRECTION ( 'NONE',  ( -1.000000000000000000, 0.000000000000000000, 0.000000000000000000 ) ) ;
#16092 = AXIS2_PLACEMENT_3D ( 'NONE', #21971, #8320, #6877 ) ;
#16093 = ORIENTED_EDGE ( 'NONE', *, *, #10910, .T. ) ;
#16094 = ORIENTED_EDGE ( 'NONE', *, *, #3210, .T. ) ;
#16095 = LINE ( 'NONE', #20039, #2039 ) ;
#16096 = APPLICATION_PROTOCOL_DEFINITION ( 'draft international standard', 'automotive_design', 1998, #15306 ) ;
#16097 = ORIENTED_EDGE ( 'NONE', *, *, #13410, .T. ) ;
#16098 = ORIENTED_EDGE ( 'NONE', *, *, #9196, .F. ) ;
#16099 = CARTESIAN_POINT ( 'NONE',  ( -8.638906393579159015, 41.42245079618239600, 68.06527860057354928 ) ) ;
#16100 = EDGE_LOOP ( 'NONE', ( #20004, #12314, #8257, #13721 ) ) ;
#16101 = CARTESIAN_POINT ( 'NONE',  ( 34.69999999999998863, -84.70000000000001705, 80.00000000000000000 ) ) ;
#16102 = AXIS2_PLACEMENT_3D ( 'NONE', #21709, #13799, #10368 ) ;
#16103 = DIRECTION ( 'NONE',  ( 0.000000000000000000, 0.000000000000000000, 1.000000000000000000 ) ) ;
#16104 = EDGE_CURVE ( 'NONE', #12460, #6564, #11641, .T. ) ;
#16105 = DIRECTION ( 'NONE',  ( 0.000000000000000000, 0.000000000000000000, 1.000000000000000000 ) ) ;
#16106 = AXIS2_PLACEMENT_3D ( 'NONE', #4813, #9971, #20257 ) ;
#16107 = EDGE_CURVE ( 'NONE', #13680, #10431, #7763, .T. ) ;
#16108 = CARTESIAN_POINT ( 'NONE',  ( 29.50000000000002132, -69.00000000000000000, 0.2999999999999947153 ) ) ;
#16109 = CARTESIAN_POINT ( 'NONE',  ( -15.21174975910705207, -41.81054587065082728, 68.50000000000000000 ) ) ;
#16110 = AXIS2_PLACEMENT_3D ( 'NONE', #3860, #10683, #17499 ) ;
#16111 = FACE_OUTER_BOUND ( 'NONE', #8107, .T. ) ;
#16112 = AXIS2_PLACEMENT_3D ( 'NONE', #21871, #8422, #4964 ) ;
#16113 = DIRECTION ( 'NONE',  ( 0.2309407893632113573, -0.9729678061520313781, -0.000000000000000000 ) ) ;
#16114 = AXIS2_PLACEMENT_3D ( 'NONE', #13960, #20705, #5494 ) ;
#16115 =( BOUNDED_SURFACE ( )  B_SPLINE_SURFACE ( 3, 2, ( 
 ( #7293, #21062, #14206 ),
 ( #19264, #12191, #12410 ),
 ( #19044, #10529, #7080 ),
 ( #19144, #443, #3708 ),
 ( #12090, #14087, #2015 ),
 ( #20936, #8969, #2348 ),
 ( #340, #7403, #5744 ),
 ( #1908, #15545, #10855 ),
 ( #8748, #13877, #19372 ),
 ( #10758, #15988, #12521 ),
 ( #3822, #2241, #3940 ),
 ( #222, #20726, #10643 ) ),
 .UNSPECIFIED., .F., .F., .F. ) 
 B_SPLINE_SURFACE_WITH_KNOTS ( ( 4, 2, 2, 2, 2, 4 ),
 ( 3, 3 ),
 ( 0.0006083281319963866878, 0.001004469391314930567, 0.001400610650633474664, 0.001796751909952018760, 0.001994822539611290808, 0.002192893169270562857 ),
 ( 0.000000000000000000, 1.000000000000000000 ),
 .UNSPECIFIED. ) 
 GEOMETRIC_REPRESENTATION_ITEM ( )  RATIONAL_B_SPLINE_SURFACE ( (
 ( 1.000000000000000000, 0.7071067811865475727, 1.000000000000000000),
 ( 1.000000000000000000, 0.7419362082869460640, 1.000000000000000000),
 ( 1.000000000000000000, 0.7734000586050232551, 1.000000000000000000),
 ( 1.000000000000000000, 0.8313348272087556223, 1.000000000000000000),
 ( 1.000000000000000000, 0.8578042680912326690, 1.000000000000000000),
 ( 1.000000000000000000, 0.9064979099737223711, 1.000000000000000000),
 ( 1.000000000000000000, 0.9284078965777988746, 1.000000000000000000),
 ( 1.000000000000000000, 0.9565959158316886812, 1.000000000000000000),
 ( 1.000000000000000000, 0.9652268734598682398, 1.000000000000000000),
 ( 1.000000000000000000, 0.9789818400845352597, 1.000000000000000000),
 ( 1.000000000000000000, 0.9843224408025195160, 1.000000000000000000),
 ( 1.000000000000000000, 0.9842566880020492404, 1.000000000000000000) ) ) 
 REPRESENTATION_ITEM ( '' )  SURFACE ( )  );
#16116 = CARTESIAN_POINT ( 'NONE',  ( 1.724728116533979838, 43.26054587065083012, 29.66679706732590560 ) ) ;
#16117 = EDGE_LOOP ( 'NONE', ( #10825, #9316, #18613, #22013, #21925, #20889 ) ) ;
#16118 = ORIENTED_EDGE ( 'NONE', *, *, #1093, .F. ) ;
#16119 = CARTESIAN_POINT ( 'NONE',  ( 0.000000000000000000, 43.26054587065083012, 39.75876104995654003 ) ) ;
#16120 = SURFACE_STYLE_USAGE ( .BOTH. , #14105 ) ;
#16121 = PRODUCT_DEFINITION ( 'UNKNOWN', '', #3721, #3803 ) ;
#16122 = ORIENTED_EDGE ( 'NONE', *, *, #11046, .F. ) ;
#16123 = CIRCLE ( 'NONE', #8300, 0.05000000000000143219 ) ;
#16124 = CIRCLE ( 'NONE', #2574, 0.5000000000000004441 ) ;
#16125 = CARTESIAN_POINT ( 'NONE',  ( 27.37540678000427974, -5.683640910026986681, 13.79999999999999893 ) ) ;
#16126 = VECTOR ( 'NONE', #11162, 1000.000000000000000 ) ;
#16127 = EDGE_CURVE ( 'NONE', #12714, #9336, #9321, .T. ) ;
#16128 = AXIS2_PLACEMENT_3D ( 'NONE', #13477, #15267, #6796 ) ;
#16129 = DIRECTION ( 'NONE',  ( 0.000000000000000000, 0.000000000000000000, 1.000000000000000000 ) ) ;
#16130 = VERTEX_POINT ( 'NONE', #14444 ) ;
#16131 = LINE ( 'NONE', #14117, #2494 ) ;
#16132 = FACE_OUTER_BOUND ( 'NONE', #3424, .T. ) ;
#16133 = CARTESIAN_POINT ( 'NONE',  ( -28.82574430125643516, 6.542305536751587880, 13.37088755551135932 ) ) ;
#16134 = CARTESIAN_POINT ( 'NONE',  ( -14.66174975910704781, 51.84664399969958737, 13.49999999999999645 ) ) ;
#16135 = CARTESIAN_POINT ( 'NONE',  ( 33.19999999999999574, -85.00000000000000000, 78.79999999999999716 ) ) ;
#16136 = ORIENTED_EDGE ( 'NONE', *, *, #20246, .T. ) ;
#16137 = DIRECTION ( 'NONE',  ( 1.000000000000000000, 0.000000000000000000, 0.000000000000000000 ) ) ;
#16138 = CARTESIAN_POINT ( 'NONE',  ( -1.724728116533986721, 43.26054587065083012, 51.70876104995653577 ) ) ;
#16139 = ORIENTED_EDGE ( 'NONE', *, *, #4365, .T. ) ;
#16140 = VERTEX_POINT ( 'NONE', #21642 ) ;
#16141 = VERTEX_POINT ( 'NONE', #9433 ) ;
#16142 = LINE ( 'NONE', #15920, #12732 ) ;
#16143 = AXIS2_PLACEMENT_3D ( 'NONE', #12074, #7387, #19356 ) ;
#16144 = DIRECTION ( 'NONE',  ( 1.000000000000000000, 0.000000000000000000, 0.000000000000000000 ) ) ;
#16145 = ORIENTED_EDGE ( 'NONE', *, *, #14065, .T. ) ;
#16146 = AXIS2_PLACEMENT_3D ( 'NONE', #5359, #15177, #18998 ) ;
#16147 = EDGE_CURVE ( 'NONE', #2496, #20277, #13790, .T. ) ;
#16148 = CARTESIAN_POINT ( 'NONE',  ( -32.23382792203229741, 83.71979900898287497, 68.50000000000000000 ) ) ;
#16149 = ORIENTED_EDGE ( 'NONE', *, *, #19060, .F. ) ;
#16150 = DIRECTION ( 'NONE',  ( -0.000000000000000000, 1.000000000000000000, -0.000000000000000000 ) ) ;
#16151 = CARTESIAN_POINT ( 'NONE',  ( -28.87540678000427619, 0.000000000000000000, 7.799999999999999822 ) ) ;
#16152 = AXIS2_PLACEMENT_3D ( 'NONE', #17352, #7094, #14096 ) ;
#16153 = EDGE_CURVE ( 'NONE', #13818, #4728, #582, .T. ) ;
#16154 = CARTESIAN_POINT ( 'NONE',  ( -17.45292532278785913, -34.11873716947361856, 68.00000000000000000 ) ) ;
#16155 = FACE_OUTER_BOUND ( 'NONE', #12506, .T. ) ;
#16156 = DIRECTION ( 'NONE',  ( 1.000000000000000000, 0.000000000000000000, -2.388292521039847891E-16 ) ) ;
#16157 = DIRECTION ( 'NONE',  ( -1.000000000000000000, 0.000000000000000000, 0.000000000000000000 ) ) ;
#16158 = ORIENTED_EDGE ( 'NONE', *, *, #21452, .T. ) ;
#16159 = DIRECTION ( 'NONE',  ( 0.000000000000000000, -1.000000000000000000, 0.000000000000000000 ) ) ;
#16160 = DIRECTION ( 'NONE',  ( 0.000000000000000000, -1.000000000000000000, 0.000000000000000000 ) ) ;
#16161 = DIRECTION ( 'NONE',  ( -1.000000000000000000, 0.000000000000000000, 0.000000000000000000 ) ) ;
#16162 = CARTESIAN_POINT ( 'NONE',  ( -23.04273156199909423, -2.261510999192741345, 13.22936009151389847 ) ) ;
#16163 = ORIENTED_EDGE ( 'NONE', *, *, #16798, .F. ) ;
#16164 = CARTESIAN_POINT ( 'NONE',  ( -15.21174975910705207, 52.39333383871510108, 13.79999999999999893 ) ) ;
#16165 = DIRECTION ( 'NONE',  ( 0.000000000000000000, 0.000000000000000000, -1.000000000000000000 ) ) ;
#16166 = ORIENTED_EDGE ( 'NONE', *, *, #14440, .F. ) ;
#16167 = CARTESIAN_POINT ( 'NONE',  ( -31.44597781366222122, 56.94165929845684815, 68.50000000000000000 ) ) ;
#16168 = CARTESIAN_POINT ( 'NONE',  ( -33.80000000000000426, -85.00000000000000000, -5.863365348801607979E-15 ) ) ;
#16169 = EDGE_LOOP ( 'NONE', ( #17971, #13069, #11857, #2150, #4840, #8439 ) ) ;
#16170 = ORIENTED_EDGE ( 'NONE', *, *, #15899, .F. ) ;
#16171 = FACE_BOUND ( 'NONE', #16836, .T. ) ;
#16172 = DIRECTION ( 'NONE',  ( -1.000000000000000000, 0.000000000000000000, 0.000000000000000000 ) ) ;
#16173 = EDGE_CURVE ( 'NONE', #15775, #10812, #3467, .T. ) ;
#16174 = CARTESIAN_POINT ( 'NONE',  ( 26.37540678000427619, -10.94079601157914716, 13.79999999999999893 ) ) ;
#16175 = ORIENTED_EDGE ( 'NONE', *, *, #6878, .F. ) ;
#16176 = ORIENTED_EDGE ( 'NONE', *, *, #3698, .F. ) ;
#16177 = CARTESIAN_POINT ( 'NONE',  ( 1.724728116533979616, 43.26054587065083012, 51.80876104995653719 ) ) ;
#16178 = EDGE_CURVE ( 'NONE', #8747, #4728, #15242, .T. ) ;
#16179 = ADVANCED_FACE ( 'NONE', ( #19840 ), #16361, .T. ) ;
#16180 = ORIENTED_EDGE ( 'NONE', *, *, #5559, .F. ) ;
#16181 = LINE ( 'NONE', #10736, #3848 ) ;
#16182 = EDGE_CURVE ( 'NONE', #18705, #12963, #6203, .T. ) ;
#16183 = DIRECTION ( 'NONE',  ( -2.107255972849994642E-16, 0.000000000000000000, -1.000000000000000000 ) ) ;
#16184 = CARTESIAN_POINT ( 'NONE',  ( -3.627054932750481964, 33.93424481021354921, 68.50000000000000000 ) ) ;
#16185 = EDGE_CURVE ( 'NONE', #9364, #8265, #19965, .T. ) ;
#16186 = CARTESIAN_POINT ( 'NONE',  ( -10.05825507651049655, 41.92645089659917801, 69.00503344894293889 ) ) ;
#16187 = CARTESIAN_POINT ( 'NONE',  ( 0.000000000000000000, 42.31054587065082728, 27.75876104995654003 ) ) ;
#16188 = AXIS2_PLACEMENT_3D ( 'NONE', #13431, #20273, #3265 ) ;
#16189 = ORIENTED_EDGE ( 'NONE', *, *, #15707, .F. ) ;
#16190 = CYLINDRICAL_SURFACE ( 'NONE', #5927, 0.04999999999999991257 ) ;
#16191 = CARTESIAN_POINT ( 'NONE',  ( 31.69597781366222122, 27.99124249474150972, 70.25000000000000000 ) ) ;
#16192 = DIRECTION ( 'NONE',  ( -0.000000000000000000, -1.000000000000000000, -0.000000000000000000 ) ) ;
#16193 = EDGE_CURVE ( 'NONE', #17942, #2242, #12372, .T. ) ;
#16195 = VECTOR ( 'NONE', #9252, 1000.000000000000114 ) ;
#16194 = CARTESIAN_POINT ( 'NONE',  ( -14.96174975910705207, -41.81054587065082728, 68.25000000000000000 ) ) ;
#16196 = ORIENTED_EDGE ( 'NONE', *, *, #12652, .F. ) ;
#16197 = EDGE_LOOP ( 'NONE', ( #9662, #15501, #5718, #11755 ) ) ;
#16198 = ORIENTED_EDGE ( 'NONE', *, *, #1784, .T. ) ;
#16199 = DIRECTION ( 'NONE',  ( 0.000000000000000000, 0.000000000000000000, -1.000000000000000000 ) ) ;
#16200 = ORIENTED_EDGE ( 'NONE', *, *, #19476, .F. ) ;
#16201 = AXIS2_PLACEMENT_3D ( 'NONE', #3256, #1339, #11854 ) ;
#16202 = ORIENTED_EDGE ( 'NONE', *, *, #439, .F. ) ;
#16203 = ORIENTED_EDGE ( 'NONE', *, *, #20183, .F. ) ;
#16204 = LINE ( 'NONE', #19466, #2579 ) ;
#16205 = ORIENTED_EDGE ( 'NONE', *, *, #15085, .T. ) ;
#16206 = DIRECTION ( 'NONE',  ( -0.000000000000000000, 1.000000000000000000, 0.000000000000000000 ) ) ;
#16207 = EDGE_CURVE ( 'NONE', #1590, #9618, #5622, .T. ) ;
#16208 = VERTEX_POINT ( 'NONE', #17805 ) ;
#16209 = EDGE_CURVE ( 'NONE', #2496, #1170, #12028, .T. ) ;
#16210 = DIRECTION ( 'NONE',  ( -0.000000000000000000, 1.000000000000000000, -0.000000000000000000 ) ) ;
#16211 = DIRECTION ( 'NONE',  ( 0.000000000000000000, 0.000000000000000000, -1.000000000000000000 ) ) ;
#16212 = DIRECTION ( 'NONE',  ( 1.000000000000000000, -0.000000000000000000, -0.000000000000000000 ) ) ;
#16213 = DIRECTION ( 'NONE',  ( -0.000000000000000000, -1.000000000000000000, -0.000000000000000000 ) ) ;
#16214 = DIRECTION ( 'NONE',  ( 0.000000000000000000, 0.000000000000000000, 1.000000000000000000 ) ) ;
#16215 = DIRECTION ( 'NONE',  ( 1.000000000000000000, 0.000000000000000000, 0.000000000000000000 ) ) ;
#16216 = FACE_BOUND ( 'NONE', #10665, .T. ) ;
#16217 = CARTESIAN_POINT ( 'NONE',  ( -9.641460742840918030, -32.93424481021354921, 68.50000000000000000 ) ) ;
#16218 = LINE ( 'NONE', #4385, #21016 ) ;
#16219 = VERTEX_POINT ( 'NONE', #16217 ) ;
#16220 = ORIENTED_EDGE ( 'NONE', *, *, #606, .F. ) ;
#16221 = CARTESIAN_POINT ( 'NONE',  ( -15.21174975910705207, 42.31054587065082728, 13.50000000000000000 ) ) ;
#16222 = SURFACE_STYLE_USAGE ( .BOTH. , #9423 ) ;
#16224 = EDGE_CURVE ( 'NONE', #8987, #4526, #16457, .T. ) ;
#16223 = DIRECTION ( 'NONE',  ( -1.000000000000000000, 0.000000000000000000, 0.000000000000000000 ) ) ;
#16225 = ORIENTED_EDGE ( 'NONE', *, *, #5750, .F. ) ;
#16226 = DIRECTION ( 'NONE',  ( 1.000000000000000000, 0.000000000000000000, 0.000000000000000000 ) ) ;
#16227 = ORIENTED_EDGE ( 'NONE', *, *, #114, .F. ) ;
#16228 = CIRCLE ( 'NONE', #21265, 2.000000000000001776 ) ;
#16229 = ADVANCED_FACE ( 'NONE', ( #13091 ), #11195, .T. ) ;
#16230 = DIRECTION ( 'NONE',  ( 0.000000000000000000, 1.000000000000000000, -0.000000000000000000 ) ) ;
#16231 = DIRECTION ( 'NONE',  ( -1.000000000000000000, 0.000000000000000000, 0.000000000000000000 ) ) ;
#16232 = ORIENTED_EDGE ( 'NONE', *, *, #9663, .F. ) ;
#16233 = CARTESIAN_POINT ( 'NONE',  ( -8.638906393579159015, 40.01645089659919563, 70.88527860057354246 ) ) ;
#16234 = LINE ( 'NONE', #7891, #5070 ) ;
#16235 = DIRECTION ( 'NONE',  ( 0.000000000000000000, 1.000000000000000000, 0.000000000000000000 ) ) ;
#16236 = DIRECTION ( 'NONE',  ( -0.000000000000000000, 0.000000000000000000, 1.000000000000000000 ) ) ;
#16237 = CARTESIAN_POINT ( 'NONE',  ( 1.724728116533979616, 42.31054587065082728, 33.71679706732589921 ) ) ;
#16238 = ORIENTED_EDGE ( 'NONE', *, *, #5487, .T. ) ;
#16239 = CARTESIAN_POINT ( 'NONE',  ( -29.20000000000002061, 50.00000000000000000, 0.000000000000000000 ) ) ;
#16240 = FACE_OUTER_BOUND ( 'NONE', #17662, .T. ) ;
#16241 = VERTEX_POINT ( 'NONE', #2692 ) ;
#16242 = AXIS2_PLACEMENT_3D ( 'NONE', #6804, #13603, #16733 ) ;
#16243 = VERTEX_POINT ( 'NONE', #11424 ) ;
#16244 = AXIS2_PLACEMENT_3D ( 'NONE', #21346, #6238, #16403 ) ;
#16245 = VERTEX_POINT ( 'NONE', #4614 ) ;
#16246 = DIRECTION ( 'NONE',  ( 1.000000000000000000, 0.000000000000000000, 0.000000000000000000 ) ) ;
#16248 = ADVANCED_FACE ( 'NONE', ( #16340 ), #21190, .F. ) ;
#16247 = DIRECTION ( 'NONE',  ( 0.9969624470112576908, -0.07788375472025980961, -0.000000000000000000 ) ) ;
#16249 = ORIENTED_EDGE ( 'NONE', *, *, #20888, .T. ) ;
#16250 = ADVANCED_FACE ( 'NONE', ( #19949 ), #17375, .T. ) ;
#16251 = DIRECTION ( 'NONE',  ( 0.000000000000000000, 1.000000000000000000, 0.000000000000000000 ) ) ;
#16252 = ORIENTED_EDGE ( 'NONE', *, *, #21586, .F. ) ;
#16253 = CARTESIAN_POINT ( 'NONE',  ( 14.83748569039512866, -41.93480993936275780, 13.49999999999999822 ) ) ;
#16254 = CYLINDRICAL_SURFACE ( 'NONE', #10615, 2.000000000000001776 ) ;
#16255 = CARTESIAN_POINT ( 'NONE',  ( -14.96174975910705207, 42.31054587065082728, 13.75000000000000000 ) ) ;
#16256 = DIRECTION ( 'NONE',  ( -1.000000000000000000, 0.000000000000000000, 0.000000000000000000 ) ) ;
#16257 = CIRCLE ( 'NONE', #12326, 0.2999999999999999334 ) ;
#16258 = CARTESIAN_POINT ( 'NONE',  ( -8.638906393579159015, 43.51045099701597252, 68.06527860057354928 ) ) ;
#16259 = AXIS2_PLACEMENT_3D ( 'NONE', #1396, #15054, #4878 ) ;
#16260 = CARTESIAN_POINT ( 'NONE',  ( 1.824728116533979261, 42.36054587065083155, 39.80876104995653719 ) ) ;
#16261 = ORIENTED_EDGE ( 'NONE', *, *, #3509, .T. ) ;
#16262 = DIRECTION ( 'NONE',  ( 1.000000000000000000, 0.000000000000000000, 0.000000000000000000 ) ) ;
#16263 = CARTESIAN_POINT ( 'NONE',  ( -30.07540678000427548, 0.000000000000000000, 7.200000000000000178 ) ) ;
#16264 = CARTESIAN_POINT ( 'NONE',  ( 25.37540678000429040, -36.74634676501047181, 13.79999999999999893 ) ) ;
#16265 = CARTESIAN_POINT ( 'NONE',  ( -26.61833302554978786, 9.663695060508649348, 13.50000000000000000 ) ) ;
#16266 = EDGE_LOOP ( 'NONE', ( #20496, #3430, #5757, #18564 ) ) ;
#16267 = ADVANCED_FACE ( 'NONE', ( #21523 ), #14551, .F. ) ;
#16268 = DIRECTION ( 'NONE',  ( 1.000000000000000000, 0.000000000000000000, 6.123233995736766036E-17 ) ) ;
#16269 = DIRECTION ( 'NONE',  ( -0.000000000000000000, -1.000000000000000000, -0.000000000000000000 ) ) ;
#16270 = ORIENTED_EDGE ( 'NONE', *, *, #10506, .T. ) ;
#16271 = DIRECTION ( 'NONE',  ( 1.000000000000000000, 0.000000000000000000, 0.000000000000000000 ) ) ;
#16272 = CARTESIAN_POINT ( 'NONE',  ( -29.37540678000427619, 5.000000000000000000, 7.200000000000000178 ) ) ;
#16273 = ORIENTED_EDGE ( 'NONE', *, *, #15925, .F. ) ;
#16274 = VECTOR ( 'NONE', #10156, 1000.000000000000000 ) ;
#16275 = AXIS2_PLACEMENT_3D ( 'NONE', #14976, #18555, #22038 ) ;
#16276 = AXIS2_PLACEMENT_3D ( 'NONE', #19759, #1062, #2740 ) ;
#16277 = ORIENTED_EDGE ( 'NONE', *, *, #4313, .F. ) ;
#16278 = DIRECTION ( 'NONE',  ( 1.000000000000000000, 0.000000000000000000, 0.000000000000000000 ) ) ;
#16279 = DIRECTION ( 'NONE',  ( -1.224646799147353207E-16, -0.000000000000000000, -1.000000000000000000 ) ) ;
#16280 = EDGE_CURVE ( 'NONE', #12981, #1863, #18100, .T. ) ;
#16281 = CARTESIAN_POINT ( 'NONE',  ( -31.31859531322107060, 84.19398174988410233, 68.25000000000000000 ) ) ;
#16282 = AXIS2_PLACEMENT_3D ( 'NONE', #14652, #21617, #6279 ) ;
#16283 = ORIENTED_EDGE ( 'NONE', *, *, #1182, .T. ) ;
#16284 = AXIS2_PLACEMENT_3D ( 'NONE', #16937, #11787, #1604 ) ;
#16285 = EDGE_LOOP ( 'NONE', ( #4826, #3038, #4519, #5760 ) ) ;
#16286 = DIRECTION ( 'NONE',  ( 2.105859220307292343E-16, -1.000000000000000000, 0.000000000000000000 ) ) ;
#16287 = FACE_OUTER_BOUND ( 'NONE', #10852, .T. ) ;
#16288 = FACE_OUTER_BOUND ( 'NONE', #669, .T. ) ;
#16289 = CIRCLE ( 'NONE', #14879, 1.499999999999999556 ) ;
#16290 = AXIS2_PLACEMENT_3D ( 'NONE', #6137, #959, #12928 ) ;
#16291 = DIRECTION ( 'NONE',  ( 1.000000000000000000, 0.000000000000000000, 0.000000000000000000 ) ) ;
#16292 = AXIS2_PLACEMENT_3D ( 'NONE', #11387, #13280, #6374 ) ;
#16293 = DIRECTION ( 'NONE',  ( 0.000000000000000000, 1.000000000000000000, 0.000000000000000000 ) ) ;
#16294 = DIRECTION ( 'NONE',  ( 0.000000000000000000, -0.000000000000000000, -1.000000000000000000 ) ) ;
#16295 = EDGE_CURVE ( 'NONE', #19855, #10953, #7748, .T. ) ;
#16296 = LINE ( 'NONE', #14746, #21348 ) ;
#16297 = DIRECTION ( 'NONE',  ( -1.038507728162729346E-16, -1.000000000000000000, 1.271805165184275985E-32 ) ) ;
#16298 = ORIENTED_EDGE ( 'NONE', *, *, #10220, .F. ) ;
#16299 = DIRECTION ( 'NONE',  ( -0.000000000000000000, -0.000000000000000000, -1.000000000000000000 ) ) ;
#16300 = AXIS2_PLACEMENT_3D ( 'NONE', #18355, #4943, #10196 ) ;
#16301 = DIRECTION ( 'NONE',  ( 0.000000000000000000, 0.000000000000000000, -1.000000000000000000 ) ) ;
#16302 = DIRECTION ( 'NONE',  ( 1.000000000000000000, 0.000000000000000000, 0.000000000000000000 ) ) ;
#16303 = DIRECTION ( 'NONE',  ( 1.000000000000000000, 0.000000000000000000, 0.000000000000000000 ) ) ;
#16304 = EDGE_CURVE ( 'NONE', #7942, #3680, #18253, .T. ) ;
#16305 = EDGE_CURVE ( 'NONE', #4651, #124, #12868, .T. ) ;
#16306 = DIRECTION ( 'NONE',  ( -1.000000000000000000, 3.009265538104883829E-28, -4.336808689941893885E-15 ) ) ;
#16307 = ORIENTED_EDGE ( 'NONE', *, *, #8421, .F. ) ;
#16308 = VECTOR ( 'NONE', #579, 1000.000000000000000 ) ;
#16309 = EDGE_CURVE ( 'NONE', #857, #7850, #7402, .T. ) ;
#16310 = CIRCLE ( 'NONE', #18460, 0.2500000000000002220 ) ;
#16311 = CIRCLE ( 'NONE', #8844, 0.05000000000000143219 ) ;
#16312 = VERTEX_POINT ( 'NONE', #19483 ) ;
#16313 = FACE_OUTER_BOUND ( 'NONE', #22075, .T. ) ;
#16314 = AXIS2_PLACEMENT_3D ( 'NONE', #15416, #10058, #13394 ) ;
#16315 = ADVANCED_BREP_SHAPE_REPRESENTATION ( '', ( #20415, #17493 ), #19794 ) ;
#16316 = ORIENTED_EDGE ( 'NONE', *, *, #19901, .T. ) ;
#16317 = CIRCLE ( 'NONE', #12387, 0.3000000000000004885 ) ;
#16318 = LINE ( 'NONE', #21389, #12201 ) ;
#16319 = ORIENTED_EDGE ( 'NONE', *, *, #21253, .T. ) ;
#16320 = FACE_OUTER_BOUND ( 'NONE', #14607, .T. ) ;
#16321 = ORIENTED_EDGE ( 'NONE', *, *, #15703, .F. ) ;
#16322 = DIRECTION ( 'NONE',  ( 0.000000000000000000, 1.000000000000000000, 0.000000000000000000 ) ) ;
#16323 = DIRECTION ( 'NONE',  ( -0.000000000000000000, 0.000000000000000000, 1.000000000000000000 ) ) ;
#16324 = EDGE_CURVE ( 'NONE', #11318, #12310, #2380, .T. ) ;
#16325 = CARTESIAN_POINT ( 'NONE',  ( -1.774728116533986766, 42.36054587065083155, 51.70876104995653577 ) ) ;
#16326 = CLOSED_SHELL ( 'NONE', ( #19614, #3944, #12190, #1111, #10283, #3715, #3749, #2681, #20288, #12630, #12440, #19540, #9034, #22077, #16501, #11662, #10595, #15681, #10409, #11920, #11439, #4608, #17688, #12992, #2491, #19092, #18756, #760, #4996, #18897, #13082, #19088, #15604, #15825, #7529, #19242, #3634, #1568, #11939, #11569, #1727, #2041 ) ) ;
#16327 = VECTOR ( 'NONE', #17981, 1000.000000000000000 ) ;
#16328 = TOROIDAL_SURFACE ( 'NONE', #9913, 0.05000000000000000278, 0.05000000000000000278 ) ;
#16329 = CARTESIAN_POINT ( 'NONE',  ( 23.04273156199908357, 2.261510999192738680, 13.19999999999999929 ) ) ;
#16330 = FACE_OUTER_BOUND ( 'NONE', #10038, .T. ) ;
#16331 = CARTESIAN_POINT ( 'NONE',  ( -1.824728116533986810, 43.26054587065083012, 47.80876104995653719 ) ) ;
#16332 = AXIS2_PLACEMENT_3D ( 'NONE', #491, #13814, #14141 ) ;
#16333 = FACE_OUTER_BOUND ( 'NONE', #3090, .T. ) ;
#16334 = CARTESIAN_POINT ( 'NONE',  ( 1.724728116533979616, 43.26054587065083012, 43.80876104995653719 ) ) ;
#16335 = CARTESIAN_POINT ( 'NONE',  ( -14.71174975910705029, 52.11873716947361856, 68.00000000000000000 ) ) ;
#16336 = AXIS2_PLACEMENT_3D ( 'NONE', #20878, #10899, #14362 ) ;
#16337 = CIRCLE ( 'NONE', #3853, 0.2500000000000002220 ) ;
#16338 = EDGE_CURVE ( 'NONE', #9421, #20875, #19604, .T. ) ;
#16339 = ORIENTED_EDGE ( 'NONE', *, *, #16843, .T. ) ;
#16340 = FACE_OUTER_BOUND ( 'NONE', #17202, .T. ) ;
#16341 = EDGE_CURVE ( 'NONE', #19370, #9810, #20969, .T. ) ;
#16342 = FACE_OUTER_BOUND ( 'NONE', #16753, .T. ) ;
#16343 = VERTEX_POINT ( 'NONE', #5964 ) ;
#16344 = ORIENTED_EDGE ( 'NONE', *, *, #6834, .F. ) ;
#16345 = LINE ( 'NONE', #1023, #12766 ) ;
#16346 = EDGE_CURVE ( 'NONE', #22161, #18590, #3096, .T. ) ;
#16347 = CARTESIAN_POINT ( 'NONE',  ( -33.20000000000001705, -85.00000000000000000, 78.79999999999999716 ) ) ;
#16348 = ORIENTED_EDGE ( 'NONE', *, *, #1473, .F. ) ;
#16349 = ORIENTED_EDGE ( 'NONE', *, *, #543, .F. ) ;
#16350 = CIRCLE ( 'NONE', #4206, 0.2999999999999999334 ) ;
#16351 = AXIS2_PLACEMENT_3D ( 'NONE', #11786, #16716, #3636 ) ;
#16352 = AXIS2_PLACEMENT_3D ( 'NONE', #17754, #19013, #3910 ) ;
#16353 = DIRECTION ( 'NONE',  ( -0.000000000000000000, 1.000000000000000000, -0.000000000000000000 ) ) ;
#16354 = ORIENTED_EDGE ( 'NONE', *, *, #20928, .F. ) ;
#16355 = CIRCLE ( 'NONE', #7805, 1.499999999999999556 ) ;
#16356 = VECTOR ( 'NONE', #20395, 1000.000000000000000 ) ;
#16357 = ORIENTED_EDGE ( 'NONE', *, *, #1972, .F. ) ;
#16358 = AXIS2_PLACEMENT_3D ( 'NONE', #173, #5128, #3437 ) ;
#16359 = EDGE_CURVE ( 'NONE', #13238, #20804, #11965, .T. ) ;
#16360 = CARTESIAN_POINT ( 'NONE',  ( 15.21174975910705918, -52.10286008774955491, 13.87500000000000000 ) ) ;
#16361 = PLANE ( 'NONE',  #22054 ) ;
#16362 = ORIENTED_EDGE ( 'NONE', *, *, #14872, .T. ) ;
#16363 = CARTESIAN_POINT ( 'NONE',  ( 4.985331397971318523, 42.46645089659917716, 70.50000000000000000 ) ) ;
#16364 = EDGE_CURVE ( 'NONE', #17313, #13197, #3481, .T. ) ;
#16365 = DIRECTION ( 'NONE',  ( 1.000000000000000000, 0.000000000000000000, -0.000000000000000000 ) ) ;
#16366 = CARTESIAN_POINT ( 'NONE',  ( 15.21174975910705918, 52.39333383871510108, 13.50000000000000000 ) ) ;
#16367 = DIRECTION ( 'NONE',  ( 0.000000000000000000, -1.000000000000000000, 0.000000000000000000 ) ) ;
#16368 = AXIS2_PLACEMENT_3D ( 'NONE', #19067, #12441, #17492 ) ;
#16369 = CARTESIAN_POINT ( 'NONE',  ( -9.178906393579158163, 42.46645089659918426, 70.88527860057354246 ) ) ;
#16370 = ORIENTED_EDGE ( 'NONE', *, *, #2298, .T. ) ;
#16371 = CARTESIAN_POINT ( 'NONE',  ( 31.50000000000002132, -71.00000000000001421, 1.500000000000000000 ) ) ;
#16372 = DIRECTION ( 'NONE',  ( -0.000000000000000000, -0.000000000000000000, -1.000000000000000000 ) ) ;
#16373 = AXIS2_PLACEMENT_3D ( 'NONE', #14714, #19873, #19426 ) ;
#16374 = ORIENTED_EDGE ( 'NONE', *, *, #10798, .T. ) ;
#16375 = CIRCLE ( 'NONE', #10978, 0.2999999999999999334 ) ;
#16376 = ORIENTED_EDGE ( 'NONE', *, *, #3505, .T. ) ;
#16377 = AXIS2_PLACEMENT_3D ( 'NONE', #15660, #10427, #2236 ) ;
#16378 = ORIENTED_EDGE ( 'NONE', *, *, #9485, .T. ) ;
#16379 = CARTESIAN_POINT ( 'NONE',  ( -33.80000000000000426, -84.70000000000001705, 1.800000000000000266 ) ) ;
#16380 = AXIS2_PLACEMENT_3D ( 'NONE', #8722, #2317, #635 ) ;
#16381 = EDGE_CURVE ( 'NONE', #9400, #9364, #16790, .T. ) ;
#16382 = DIRECTION ( 'NONE',  ( 0.000000000000000000, 1.000000000000000000, 0.000000000000000000 ) ) ;
#16383 = ORIENTED_EDGE ( 'NONE', *, *, #21637, .T. ) ;
#16384 = DIRECTION ( 'NONE',  ( -0.2309407893632007824, 0.9729678061520339316, 0.000000000000000000 ) ) ;
#16385 = ORIENTED_EDGE ( 'NONE', *, *, #17666, .F. ) ;
#16386 = DIRECTION ( 'NONE',  ( 0.000000000000000000, 0.000000000000000000, 1.000000000000000000 ) ) ;
#16387 = VECTOR ( 'NONE', #6712, 1000.000000000000000 ) ;
#16388 = DIRECTION ( 'NONE',  ( 0.000000000000000000, 0.000000000000000000, 1.000000000000000000 ) ) ;
#16389 = LINE ( 'NONE', #11564, #7795 ) ;
#16390 = DIRECTION ( 'NONE',  ( -0.000000000000000000, -1.000000000000000000, 0.000000000000000000 ) ) ;
#16391 = AXIS2_PLACEMENT_3D ( 'NONE', #13911, #19072, #19178 ) ;
#16392 = DIRECTION ( 'NONE',  ( 0.000000000000000000, -0.000000000000000000, -1.000000000000000000 ) ) ;
#16393 = DIRECTION ( 'NONE',  ( 0.000000000000000000, 0.000000000000000000, 1.000000000000000000 ) ) ;
#16394 = ORIENTED_EDGE ( 'NONE', *, *, #17737, .F. ) ;
#16395 = DIRECTION ( 'NONE',  ( 0.000000000000000000, 0.000000000000000000, 1.000000000000000000 ) ) ;
#16396 = FACE_OUTER_BOUND ( 'NONE', #9892, .T. ) ;
#16397 = EDGE_CURVE ( 'NONE', #18789, #16208, #15108, .T. ) ;
#16398 = EDGE_CURVE ( 'NONE', #10410, #8471, #12005, .T. ) ;
#16399 = DIRECTION ( 'NONE',  ( -1.000000000000000000, 0.000000000000000000, 0.000000000000000000 ) ) ;
#16400 = DIRECTION ( 'NONE',  ( -1.224646799147353207E-16, 0.000000000000000000, -1.000000000000000000 ) ) ;
#16401 = ORIENTED_EDGE ( 'NONE', *, *, #6956, .T. ) ;
#16402 = EDGE_CURVE ( 'NONE', #1165, #6732, #5164, .T. ) ;
#16403 = DIRECTION ( 'NONE',  ( 0.000000000000000000, 0.000000000000000000, 1.000000000000000000 ) ) ;
#16404 = DIRECTION ( 'NONE',  ( 1.000000000000000000, 0.000000000000000000, 0.000000000000000000 ) ) ;
#16405 = VERTEX_POINT ( 'NONE', #13549 ) ;
#16406 = CARTESIAN_POINT ( 'NONE',  ( -17.45292532278785913, 0.000000000000000000, 13.99999999999999822 ) ) ;
#16407 = DIRECTION ( 'NONE',  ( 1.000000000000000000, 0.000000000000000000, 0.000000000000000000 ) ) ;
#16408 = ORIENTED_EDGE ( 'NONE', *, *, #20945, .F. ) ;
#16409 = EDGE_LOOP ( 'NONE', ( #163, #5869, #6792, #15623 ) ) ;
#16410 = DIRECTION ( 'NONE',  ( -1.000000000000000000, 0.000000000000000000, -6.123233995736764803E-17 ) ) ;
#16411 = LINE ( 'NONE', #12817, #4975 ) ;
#16412 = LINE ( 'NONE', #21582, #3865 ) ;
#16413 = AXIS2_PLACEMENT_3D ( 'NONE', #7062, #14078, #2225 ) ;
#16414 = EDGE_LOOP ( 'NONE', ( #10788, #16376, #10229, #1212 ) ) ;
#16415 = ORIENTED_EDGE ( 'NONE', *, *, #21370, .F. ) ;
#16416 = PRODUCT_RELATED_PRODUCT_CATEGORY ( 'part', '', ( #13 ) ) ;
#16417 = LINE ( 'NONE', #8037, #10765 ) ;
#16418 = DIRECTION ( 'NONE',  ( -0.000000000000000000, -1.000000000000000000, -0.000000000000000000 ) ) ;
#16419 = DIRECTION ( 'NONE',  ( 0.000000000000000000, -1.000000000000000000, 0.000000000000000000 ) ) ;
#16420 = CYLINDRICAL_SURFACE ( 'NONE', #9527, 0.5000000000000004441 ) ;
#16421 = AXIS2_PLACEMENT_3D ( 'NONE', #20539, #2052, #12226 ) ;
#16422 = CARTESIAN_POINT ( 'NONE',  ( -1.724728116533986721, 42.31054587065082728, 43.80876104995653719 ) ) ;
#16423 = LINE ( 'NONE', #20127, #7240 ) ;
#16424 = FACE_OUTER_BOUND ( 'NONE', #17978, .T. ) ;
#16425 = EDGE_CURVE ( 'NONE', #2099, #5378, #21330, .T. ) ;
#16426 = AXIS2_PLACEMENT_3D ( 'NONE', #11817, #10273, #8366 ) ;
#16427 = VECTOR ( 'NONE', #6427, 1000.000000000000000 ) ;
#16428 = AXIS2_PLACEMENT_3D ( 'NONE', #18755, #20117, #13704 ) ;
#16429 = LINE ( 'NONE', #13051, #11320 ) ;
#16430 = CARTESIAN_POINT ( 'NONE',  ( 0.000000000000000000, 32.11873716947361856, 42.50000000000000711 ) ) ;
#16431 = ORIENTED_EDGE ( 'NONE', *, *, #15014, .T. ) ;
#16432 = EDGE_CURVE ( 'NONE', #1780, #3156, #1665, .T. ) ;
#16433 = DIRECTION ( 'NONE',  ( 1.000000000000000000, 0.000000000000000000, 0.000000000000000000 ) ) ;
#16434 = CARTESIAN_POINT ( 'NONE',  ( -15.95292532278785913, -52.09333383871509682, 13.79999999999999893 ) ) ;
#16435 = DIRECTION ( 'NONE',  ( 1.000000000000000000, 0.000000000000000000, 0.000000000000000000 ) ) ;
#16436 = ORIENTED_EDGE ( 'NONE', *, *, #7123, .F. ) ;
#16437 = DIRECTION ( 'NONE',  ( -0.000000000000000000, 0.000000000000000000, 1.000000000000000000 ) ) ;
#16438 = CARTESIAN_POINT ( 'NONE',  ( 0.000000000000000000, 0.000000000000000000, 13.50000000000000000 ) ) ;
#16439 = ORIENTED_EDGE ( 'NONE', *, *, #4694, .T. ) ;
#16440 = ORIENTED_EDGE ( 'NONE', *, *, #12958, .T. ) ;
#16441 = DIRECTION ( 'NONE',  ( -1.000000000000000000, -0.000000000000000000, 0.000000000000000000 ) ) ;
#16442 = AXIS2_PLACEMENT_3D ( 'NONE', #19315, #9024, #15823 ) ;
#16443 = DIRECTION ( 'NONE',  ( 0.000000000000000000, -1.000000000000000000, 0.000000000000000000 ) ) ;
#16444 = ADVANCED_FACE ( 'NONE', ( #21955 ), #11656, .T. ) ;
#16445 = FACE_OUTER_BOUND ( 'NONE', #194, .T. ) ;
#16446 = FACE_OUTER_BOUND ( 'NONE', #12730, .T. ) ;
#16447 = DIRECTION ( 'NONE',  ( 0.000000000000000000, 0.000000000000000000, -1.000000000000000000 ) ) ;
#16448 = EDGE_CURVE ( 'NONE', #16241, #4678, #2367, .T. ) ;
#16449 = CARTESIAN_POINT ( 'NONE',  ( 18.22752199202934520, -39.04634676501046187, 13.50000000000000000 ) ) ;
#16450 = LINE ( 'NONE', #889, #16819 ) ;
#16451 = AXIS2_PLACEMENT_3D ( 'NONE', #16822, #17163, #12000 ) ;
#16452 = AXIS2_PLACEMENT_3D ( 'NONE', #19597, #2589, #11189 ) ;
#16453 = CARTESIAN_POINT ( 'NONE',  ( -1.724728116533986721, 43.26054587065083012, 53.76679706732590347 ) ) ;
#16454 = CYLINDRICAL_SURFACE ( 'NONE', #12199, 6.500000000000002665 ) ;
#16455 = CARTESIAN_POINT ( 'NONE',  ( -25.37540678000427263, -63.74634676501045050, 7.799999999999999822 ) ) ;
#16456 = ORIENTED_EDGE ( 'NONE', *, *, #21196, .T. ) ;
#16457 = LINE ( 'NONE', #1018, #8470 ) ;
#16458 = LINE ( 'NONE', #9530, #6004 ) ;
#16459 = ORIENTED_EDGE ( 'NONE', *, *, #19798, .F. ) ;
#16460 = VERTEX_POINT ( 'NONE', #1348 ) ;
#16461 = DIRECTION ( 'NONE',  ( 0.000000000000000000, 0.000000000000000000, 1.000000000000000000 ) ) ;
#16462 = DIRECTION ( 'NONE',  ( 0.000000000000000000, 0.000000000000000000, 1.000000000000000000 ) ) ;
#16463 = ADVANCED_FACE ( 'NONE', ( #6862 ), #6417, .T. ) ;
#16464 = UNCERTAINTY_MEASURE_WITH_UNIT (LENGTH_MEASURE( 1.000000000000000082E-05 ), #4219, 'distance_accuracy_value', 'NONE');
#16465 = ORIENTED_EDGE ( 'NONE', *, *, #7694, .T. ) ;
#16466 = VERTEX_POINT ( 'NONE', #20498 ) ;
#16467 = VERTEX_POINT ( 'NONE', #18805 ) ;
#16468 = VECTOR ( 'NONE', #16659, 1000.000000000000000 ) ;
#16469 = ORIENTED_EDGE ( 'NONE', *, *, #21145, .F. ) ;
#16470 = EDGE_CURVE ( 'NONE', #20293, #19133, #13452, .T. ) ;
#16471 = EDGE_CURVE ( 'NONE', #12600, #10300, #17034, .T. ) ;
#16472 = DIRECTION ( 'NONE',  ( -0.000000000000000000, 1.000000000000000000, -0.000000000000000000 ) ) ;
#16473 = EDGE_CURVE ( 'NONE', #9408, #22072, #6693, .T. ) ;
#16474 = CARTESIAN_POINT ( 'NONE',  ( 18.22752199202934520, 0.000000000000000000, 13.79999999999999893 ) ) ;
#16475 = ORIENTED_EDGE ( 'NONE', *, *, #15287, .T. ) ;
#16476 = DIRECTION ( 'NONE',  ( -0.000000000000000000, -1.000000000000000000, -0.000000000000000000 ) ) ;
#16477 = EDGE_CURVE ( 'NONE', #9561, #13657, #3366, .T. ) ;
#16478 = CIRCLE ( 'NONE', #9714, 0.05000000000000143219 ) ;
#16479 = CYLINDRICAL_SURFACE ( 'NONE', #12181, 0.2999999999999999334 ) ;
#16480 = DIRECTION ( 'NONE',  ( -1.000000000000000000, 0.000000000000000000, 0.000000000000000000 ) ) ;
#16481 = DIRECTION ( 'NONE',  ( 0.000000000000000000, 1.000000000000000000, -0.000000000000000000 ) ) ;
#16482 = ORIENTED_EDGE ( 'NONE', *, *, #8166, .F. ) ;
#16483 = CARTESIAN_POINT ( 'NONE',  ( -1.724728116533986721, 42.36054587065083155, 47.75876104995653293 ) ) ;
#16484 = ORIENTED_EDGE ( 'NONE', *, *, #21260, .F. ) ;
#16485 = ORIENTED_EDGE ( 'NONE', *, *, #11973, .F. ) ;
#16486 = VERTEX_POINT ( 'NONE', #16672 ) ;
#16487 = CARTESIAN_POINT ( 'NONE',  ( 23.32398829872514057, -2.157133568460768647, 13.50000000000000000 ) ) ;
#16488 = CARTESIAN_POINT ( 'NONE',  ( 18.22752199202934520, 39.04634676501046187, 13.50000000000000000 ) ) ;
#16489 = EDGE_CURVE ( 'NONE', #15404, #2691, #1682, .T. ) ;
#16490 = VERTEX_POINT ( 'NONE', #18468 ) ;
#16491 = DIRECTION ( 'NONE',  ( -0.000000000000000000, -0.000000000000000000, -1.000000000000000000 ) ) ;
#16492 = VECTOR ( 'NONE', #11773, 1000.000000000000000 ) ;
#16493 = VECTOR ( 'NONE', #8326, 1000.000000000000000 ) ;
#16494 = VERTEX_POINT ( 'NONE', #6529 ) ;
#16495 = CARTESIAN_POINT ( 'NONE',  ( -32.23382792203230451, 83.71979900898288918, 13.50000000000000000 ) ) ;
#16496 = DIRECTION ( 'NONE',  ( 1.000000000000000000, 0.000000000000000000, 0.000000000000000000 ) ) ;
#16497 = EDGE_CURVE ( 'NONE', #1863, #13159, #13321, .T. ) ;
#16498 = CYLINDRICAL_SURFACE ( 'NONE', #20940, 1.826718556943725202 ) ;
#16499 = ORIENTED_EDGE ( 'NONE', *, *, #9385, .F. ) ;
#16500 = CARTESIAN_POINT ( 'NONE',  ( -23.32398829872514057, -2.157133568460768647, 13.19999999999999929 ) ) ;
#16501 = ADVANCED_FACE ( 'NONE', ( #9980 ), #19667, .F. ) ;
#16502 = CARTESIAN_POINT ( 'NONE',  ( -33.20000000000001705, 84.70000000000001705, 78.20000000000000284 ) ) ;
#16503 = CARTESIAN_POINT ( 'NONE',  ( -14.96174975910705385, 51.80670431852983882, 13.81236938792781643 ) ) ;
#16504 = DIRECTION ( 'NONE',  ( 1.000000000000000000, -0.000000000000000000, 0.000000000000000000 ) ) ;
#16505 = ORIENTED_EDGE ( 'NONE', *, *, #7767, .F. ) ;
#16506 = DIRECTION ( 'NONE',  ( -3.052134192567367925E-16, -1.000000000000000000, 0.000000000000000000 ) ) ;
#16507 = FACE_OUTER_BOUND ( 'NONE', #20000, .T. ) ;
#16508 = CIRCLE ( 'NONE', #11498, 0.2999999999999999334 ) ;
#16509 = ORIENTED_EDGE ( 'NONE', *, *, #17568, .F. ) ;
#16510 = CARTESIAN_POINT ( 'NONE',  ( -1.774728116533986766, 42.36054587065083155, 39.70876104995653577 ) ) ;
#16511 = CARTESIAN_POINT ( 'NONE',  ( -23.02398829872513986, -2.623740515231446135, 13.63037280509750637 ) ) ;
#16512 = ORIENTED_EDGE ( 'NONE', *, *, #13387, .F. ) ;
#16513 = ORIENTED_EDGE ( 'NONE', *, *, #2951, .F. ) ;
#16514 = EDGE_LOOP ( 'NONE', ( #7838, #18414, #5014, #9329 ) ) ;
#16515 = CARTESIAN_POINT ( 'NONE',  ( -15.00250675241655429, 51.98442790175712247, 13.86082508289638149 ) ) ;
#16516 = DIRECTION ( 'NONE',  ( 0.000000000000000000, 0.000000000000000000, 1.000000000000000000 ) ) ;
#16517 = CARTESIAN_POINT ( 'NONE',  ( -31.69597781366222122, 58.94165929845684815, 70.50000000000000000 ) ) ;
#16518 = ORIENTED_EDGE ( 'NONE', *, *, #21271, .T. ) ;
#16519 = ADVANCED_FACE ( 'NONE', ( #2433, #8636, #16171 ), #12282, .T. ) ;
#16520 = ADVANCED_FACE ( 'NONE', ( #7069 ), #3597, .T. ) ;
#16521 = EDGE_LOOP ( 'NONE', ( #21356, #21750, #3345, #7207, #19322, #14365, #7032, #12161, #3193, #10257 ) ) ;
#16522 = CARTESIAN_POINT ( 'NONE',  ( -28.87540678000427619, 6.494748934539263274, 7.799999999999999822 ) ) ;
#16523 = CARTESIAN_POINT ( 'NONE',  ( 1.724728116533979838, 42.36054587065083155, 53.71679706732590631 ) ) ;
#16524 = CARTESIAN_POINT ( 'NONE',  ( -23.02398829872513986, -2.624244922594602514, 13.63058196926743904 ) ) ;
#16525 = DIRECTION ( 'NONE',  ( -2.107255972849994642E-16, 0.000000000000000000, -1.000000000000000000 ) ) ;
#16526 = DIRECTION ( 'NONE',  ( -0.000000000000000000, 1.000000000000000000, -0.000000000000000000 ) ) ;
#16527 = FACE_OUTER_BOUND ( 'NONE', #10700, .T. ) ;
#16528 = EDGE_CURVE ( 'NONE', #17106, #15492, #14181, .T. ) ;
#16529 = CARTESIAN_POINT ( 'NONE',  ( -23.13310673709249343, 45.37789868843801599, 13.75000000000000000 ) ) ;
#16530 = DIRECTION ( 'NONE',  ( 1.000000000000000000, -0.000000000000000000, -0.000000000000000000 ) ) ;
#16531 = FACE_OUTER_BOUND ( 'NONE', #3730, .T. ) ;
#16532 = ORIENTED_EDGE ( 'NONE', *, *, #14926, .T. ) ;
#16533 = CARTESIAN_POINT ( 'NONE',  ( 9.141460742840918030, 32.11873716947361856, 68.00000000000000000 ) ) ;
#16534 = CYLINDRICAL_SURFACE ( 'NONE', #17599, 0.05000000000000143219 ) ;
#16535 = ORIENTED_EDGE ( 'NONE', *, *, #13073, .T. ) ;
#16536 = CARTESIAN_POINT ( 'NONE',  ( 27.37540678000427619, 10.94079601157914539, 42.50000000000000000 ) ) ;
#16537 = DIRECTION ( 'NONE',  ( -1.000000000000000000, 8.031127203596333560E-16, 1.224646799147353207E-16 ) ) ;
#16538 = ORIENTED_EDGE ( 'NONE', *, *, #17756, .T. ) ;
#16539 = ORIENTED_EDGE ( 'NONE', *, *, #5563, .F. ) ;
#16540 = FACE_OUTER_BOUND ( 'NONE', #7808, .T. ) ;
#16541 = ADVANCED_FACE ( 'NONE', ( #9371 ), #10634, .F. ) ;
#16542 = ORIENTED_EDGE ( 'NONE', *, *, #10560, .T. ) ;
#16543 = ADVANCED_FACE ( 'NONE', ( #116 ), #6964, .T. ) ;
#16544 = CARTESIAN_POINT ( 'NONE',  ( -34.40000000000001279, 84.70000000000001705, 79.39999999999999147 ) ) ;
#16545 = DIRECTION ( 'NONE',  ( 0.000000000000000000, 0.000000000000000000, 1.000000000000000000 ) ) ;
#16546 = DIRECTION ( 'NONE',  ( 0.000000000000000000, 0.000000000000000000, 1.000000000000000000 ) ) ;
#16547 = CARTESIAN_POINT ( 'NONE',  ( -9.718906393579157310, 44.91645089659918710, 70.88527860057354246 ) ) ;
#16548 = CARTESIAN_POINT ( 'NONE',  ( 27.37540678000426908, 36.74634676501047181, 13.79999999999999893 ) ) ;
#16549 = LINE ( 'NONE', #14655, #14263 ) ;
#16550 = FACE_OUTER_BOUND ( 'NONE', #13099, .T. ) ;
#16551 = CARTESIAN_POINT ( 'NONE',  ( -23.02398829872513986, -3.528912754968629439, 13.79999999999999893 ) ) ;
#16552 = DIRECTION ( 'NONE',  ( 1.000000000000000000, 0.000000000000000000, 0.000000000000000000 ) ) ;
#16554 = ADVANCED_FACE ( 'NONE', ( #20603 ), #5392, .T. ) ;
#16553 = CARTESIAN_POINT ( 'NONE',  ( 29.17540678000427690, -6.499884319688664647, 7.500000000000000000 ) ) ;
#16555 = ORIENTED_EDGE ( 'NONE', *, *, #8207, .F. ) ;
#16556 = DIRECTION ( 'NONE',  ( -0.000000000000000000, -1.000000000000000000, -0.000000000000000000 ) ) ;
#16557 = EDGE_LOOP ( 'NONE', ( #12959, #16713, #12142, #10174 ) ) ;
#16558 = DIRECTION ( 'NONE',  ( 0.000000000000000000, 0.000000000000000000, 1.000000000000000000 ) ) ;
#16559 = DIRECTION ( 'NONE',  ( -0.000000000000000000, -0.000000000000000000, -1.000000000000000000 ) ) ;
#16560 = VERTEX_POINT ( 'NONE', #9262 ) ;
#16561 = ORIENTED_EDGE ( 'NONE', *, *, #5488, .T. ) ;
#16562 = CARTESIAN_POINT ( 'NONE',  ( -30.79999999999999361, -84.70000000000001705, 1.500000000000000222 ) ) ;
#16563 = EDGE_CURVE ( 'NONE', #4526, #8181, #849, .T. ) ;
#16564 = PRESENTATION_STYLE_ASSIGNMENT (( #11534 ) ) ;
#16565 = ADVANCED_FACE ( 'NONE', ( #20716 ), #10421, .F. ) ;
#16566 = ORIENTED_EDGE ( 'NONE', *, *, #19215, .T. ) ;
#16567 = CARTESIAN_POINT ( 'NONE',  ( -29.20000000000002061, 50.00000000000000000, 0.000000000000000000 ) ) ;
#16568 = ORIENTED_EDGE ( 'NONE', *, *, #4498, .T. ) ;
#16569 = VERTEX_POINT ( 'NONE', #5281 ) ;
#16570 = ORIENTED_EDGE ( 'NONE', *, *, #20663, .F. ) ;
#16571 = DIRECTION ( 'NONE',  ( 0.000000000000000000, 0.000000000000000000, -1.000000000000000000 ) ) ;
#16572 = FACE_OUTER_BOUND ( 'NONE', #11464, .T. ) ;
#16573 = AXIS2_PLACEMENT_3D ( 'NONE', #10792, #476, #18974 ) ;
#16574 = ORIENTED_EDGE ( 'NONE', *, *, #16636, .T. ) ;
#16575 = EDGE_CURVE ( 'NONE', #2571, #18470, #20826, .T. ) ;
#16576 = DIRECTION ( 'NONE',  ( 0.000000000000000000, 0.000000000000000000, 1.000000000000000000 ) ) ;
#16577 = LINE ( 'NONE', #6439, #9728 ) ;
#16578 = CARTESIAN_POINT ( 'NONE',  ( 33.49999999999998579, -84.70000000000001705, 78.20000000000000284 ) ) ;
#16579 = DIRECTION ( 'NONE',  ( 1.000000000000000000, 0.000000000000000000, 0.000000000000000000 ) ) ;
#16580 = ORIENTED_EDGE ( 'NONE', *, *, #570, .F. ) ;
#16581 = ORIENTED_EDGE ( 'NONE', *, *, #2410, .F. ) ;
#16582 = ORIENTED_EDGE ( 'NONE', *, *, #6976, .F. ) ;
#16583 = CARTESIAN_POINT ( 'NONE',  ( -29.13662752439705272, -5.000000000000000000, 7.200000000000000178 ) ) ;
#16584 = CARTESIAN_POINT ( 'NONE',  ( -29.48732477999263679, -2.488184282963944671, 0.2032176586593637813 ) ) ;
#16585 = ADVANCED_FACE ( 'NONE', ( #17231 ), #6162, .F. ) ;
#16586 = EDGE_LOOP ( 'NONE', ( #9558, #17623, #4581, #10801 ) ) ;
#16587 = ADVANCED_FACE ( 'NONE', ( #11149 ), #12931, .T. ) ;
#16588 = CARTESIAN_POINT ( 'NONE',  ( -1.724728116533986721, 42.36054587065083155, 39.70876104995653577 ) ) ;
#16589 = AXIS2_PLACEMENT_3D ( 'NONE', #10112, #8323, #14795 ) ;
#16590 = PRODUCT ( 'Glass Cover', 'Glass Cover', '', ( #2464 ) ) ;
#16591 = VERTEX_POINT ( 'NONE', #964 ) ;
#16592 = CARTESIAN_POINT ( 'NONE',  ( -29.37540678000427619, 6.000000000000000000, 3.799999999999999822 ) ) ;
#16593 = CARTESIAN_POINT ( 'NONE',  ( -17.45292532278785913, 50.11873716947361856, 68.00000000000000000 ) ) ;
#16594 = CARTESIAN_POINT ( 'NONE',  ( 23.02398829872513986, -2.280095008958279656, 13.43080372783514420 ) ) ;
#16595 = FACE_OUTER_BOUND ( 'NONE', #17266, .T. ) ;
#16596 = ORIENTED_EDGE ( 'NONE', *, *, #2142, .F. ) ;
#16597 = DIRECTION ( 'NONE',  ( 0.000000000000000000, 0.000000000000000000, -1.000000000000000000 ) ) ;
#16598 = CARTESIAN_POINT ( 'NONE',  ( 9.141460742840918030, 32.93424481021354921, 68.00000000000000000 ) ) ;
#16599 = EDGE_CURVE ( 'NONE', #6840, #10124, #22071, .T. ) ;
#16600 = DIRECTION ( 'NONE',  ( 0.000000000000000000, 0.000000000000000000, 1.000000000000000000 ) ) ;
#16601 = FACE_OUTER_BOUND ( 'NONE', #286, .T. ) ;
#16602 = EDGE_LOOP ( 'NONE', ( #17281, #15989, #7661, #6895 ) ) ;
#16603 = DIRECTION ( 'NONE',  ( -2.107255972849994642E-16, 0.000000000000000000, -1.000000000000000000 ) ) ;
#16604 = VECTOR ( 'NONE', #2641, 1000.000000000000000 ) ;
#16605 = PRESENTATION_LAYER_ASSIGNMENT (  '', '', ( #8411 ) ) ;
#16606 = DIRECTION ( 'NONE',  ( 0.000000000000000000, 0.000000000000000000, 1.000000000000000000 ) ) ;
#16607 = ORIENTED_EDGE ( 'NONE', *, *, #16879, .T. ) ;
#16608 = CARTESIAN_POINT ( 'NONE',  ( 23.04273156199908357, 2.261510999192738680, 13.19999999999999929 ) ) ;
#16609 = DIRECTION ( 'NONE',  ( 0.000000000000000000, 0.000000000000000000, 1.000000000000000000 ) ) ;
#16610 = EDGE_LOOP ( 'NONE', ( #19762, #363, #14476, #11720 ) ) ;
#16611 = ORIENTED_EDGE ( 'NONE', *, *, #21088, .F. ) ;
#16612 = VERTEX_POINT ( 'NONE', #9925 ) ;
#16613 = CARTESIAN_POINT ( 'NONE',  ( -14.90262738048940960, 52.32122554936407255, 13.50000000000000000 ) ) ;
#16614 = EDGE_CURVE ( 'NONE', #1516, #3514, #1686, .T. ) ;
#16615 = CARTESIAN_POINT ( 'NONE',  ( -29.37540678000427619, -6.000000000000000000, 7.200000000000000178 ) ) ;
#16616 = EDGE_CURVE ( 'NONE', #8285, #13360, #4675, .T. ) ;
#16617 = ORIENTED_EDGE ( 'NONE', *, *, #5532, .F. ) ;
#16618 = TOROIDAL_SURFACE ( 'NONE', #10906, 0.2500000000000000000, 0.2500000000000000000 ) ;
#16619 = EDGE_CURVE ( 'NONE', #18066, #18442, #16317, .T. ) ;
#16620 = VERTEX_POINT ( 'NONE', #13161 ) ;
#16621 = AXIS2_PLACEMENT_3D ( 'NONE', #379, #5671, #10691 ) ;
#16622 = AXIS2_PLACEMENT_3D ( 'NONE', #5874, #18159, #6208 ) ;
#16623 = AXIS2_PLACEMENT_3D ( 'NONE', #5467, #17410, #8920 ) ;
#16624 = DIRECTION ( 'NONE',  ( -1.000000000000000000, 0.000000000000000000, 0.000000000000000000 ) ) ;
#16625 = CARTESIAN_POINT ( 'NONE',  ( -23.13120573414546755, -2.711843391866163522, 13.41529098820778110 ) ) ;
#16626 = FACE_OUTER_BOUND ( 'NONE', #8313, .T. ) ;
#16627 = DIRECTION ( 'NONE',  ( 0.000000000000000000, 0.000000000000000000, 1.000000000000000000 ) ) ;
#16628 = CARTESIAN_POINT ( 'NONE',  ( -33.20000000000001705, -84.70000000000001705, 78.50000000000000000 ) ) ;
#16629 = CARTESIAN_POINT ( 'NONE',  ( 1.724728116533979616, 42.31054587065082728, 43.80876104995653719 ) ) ;
#16630 = DIRECTION ( 'NONE',  ( 1.000000000000000000, 0.000000000000000000, -2.388292521039847891E-16 ) ) ;
#16631 = LINE ( 'NONE', #6382, #1000 ) ;
#16632 = ORIENTED_EDGE ( 'NONE', *, *, #19060, .T. ) ;
#16633 = AXIS2_PLACEMENT_3D ( 'NONE', #20134, #3451, #18435 ) ;
#16634 = CARTESIAN_POINT ( 'NONE',  ( -32.29156311937309454, 83.96304096052088539, 13.49999999999999822 ) ) ;
#16635 = AXIS2_PLACEMENT_3D ( 'NONE', #15672, #18940, #8652 ) ;
#16636 = EDGE_CURVE ( 'NONE', #8198, #18, #4176, .T. ) ;
#16637 = LINE ( 'NONE', #20440, #10432 ) ;
#16638 = CARTESIAN_POINT ( 'NONE',  ( -8.638906393579159015, 41.42245079618239600, 68.06527860057354928 ) ) ;
#16639 = EDGE_LOOP ( 'NONE', ( #17717, #10849, #20362, #18752 ) ) ;
#16640 = AXIS2_PLACEMENT_3D ( 'NONE', #9747, #14765, #16546 ) ;
#16641 = AXIS2_PLACEMENT_3D ( 'NONE', #4629, #19617, #8098 ) ;
#16642 = CARTESIAN_POINT ( 'NONE',  ( -1.774728116533986766, 43.26054587065083012, 53.66679706732590915 ) ) ;
#16643 = DIRECTION ( 'NONE',  ( 0.000000000000000000, 0.000000000000000000, 1.000000000000000000 ) ) ;
#16644 = ORIENTED_EDGE ( 'NONE', *, *, #16908, .F. ) ;
#16645 = VERTEX_POINT ( 'NONE', #14949 ) ;
#16646 = CARTESIAN_POINT ( 'NONE',  ( 29.50000000000003197, -2.473451120191014763, 0.2503162269321387856 ) ) ;
#16647 = ADVANCED_FACE ( 'NONE', ( #9599 ), #7819, .T. ) ;
#16648 = ORIENTED_EDGE ( 'NONE', *, *, #9569, .F. ) ;
#16649 = CIRCLE ( 'NONE', #21302, 0.5000000000000004441 ) ;
#16650 = AXIS2_PLACEMENT_3D ( 'NONE', #10498, #21135, #2209 ) ;
#16651 = TOROIDAL_SURFACE ( 'NONE', #6687, 0.05000000000000000278, 0.05000000000000000278 ) ;
#16652 = CARTESIAN_POINT ( 'NONE',  ( -9.718906393579157310, 43.34579957953053508, 69.00503344894293889 ) ) ;
#16653 = ORIENTED_EDGE ( 'NONE', *, *, #7886, .F. ) ;
#16654 = FACE_OUTER_BOUND ( 'NONE', #125, .T. ) ;
#16655 = AXIS2_PLACEMENT_3D ( 'NONE', #9419, #2595, #1127 ) ;
#16656 = DIRECTION ( 'NONE',  ( 4.336808689941893885E-15, 0.000000000000000000, 1.000000000000000000 ) ) ;
#16657 = DIRECTION ( 'NONE',  ( 1.000000000000000000, 0.000000000000000000, 0.000000000000000000 ) ) ;
#16658 = CARTESIAN_POINT ( 'NONE',  ( 23.26721486835118569, 3.307416615798743909, 13.49999999999999645 ) ) ;
#16659 = DIRECTION ( 'NONE',  ( -1.000000000000000000, 0.000000000000000000, -0.000000000000000000 ) ) ;
#16660 = EDGE_CURVE ( 'NONE', #5066, #15826, #2760, .T. ) ;
#16661 = DIRECTION ( 'NONE',  ( 0.000000000000000000, 1.000000000000000000, 0.000000000000000000 ) ) ;
#16662 = CARTESIAN_POINT ( 'NONE',  ( -14.66174954725422630, -51.84669727004962425, 13.50000000000000000 ) ) ;
#16663 = EDGE_CURVE ( 'NONE', #18637, #5223, #7708, .T. ) ;
#16664 = AXIS2_PLACEMENT_3D ( 'NONE', #14809, #6336, #13138 ) ;
#16665 = DIRECTION ( 'NONE',  ( -0.000000000000000000, -0.000000000000000000, -1.000000000000000000 ) ) ;
#16666 = CIRCLE ( 'NONE', #10255, 1.000000000000000888 ) ;
#16667 = AXIS2_PLACEMENT_3D ( 'NONE', #4301, #5993, #11627 ) ;
#16668 = ORIENTED_EDGE ( 'NONE', *, *, #20408, .T. ) ;
#16669 = VECTOR ( 'NONE', #9945, 1000.000000000000000 ) ;
#16670 = CARTESIAN_POINT ( 'NONE',  ( -1.774728116533986766, 42.31054587065082728, 49.66679706732590915 ) ) ;
#16671 = ORIENTED_EDGE ( 'NONE', *, *, #14773, .T. ) ;
#16672 = CARTESIAN_POINT ( 'NONE',  ( -1.724728116533986721, 42.31054587065082728, 35.75876104995654003 ) ) ;
#16673 = CYLINDRICAL_SURFACE ( 'NONE', #18874, 0.3000000000000016542 ) ;
#16674 = ORIENTED_EDGE ( 'NONE', *, *, #16619, .T. ) ;
#16675 = TOROIDAL_SURFACE ( 'NONE', #3485, 1.500000000000000000, 0.5000000000000000000 ) ;
#16676 = VERTEX_POINT ( 'NONE', #21801 ) ;
#16677 = CARTESIAN_POINT ( 'NONE',  ( 14.71174975910707161, 0.000000000000000000, 68.25000000000000000 ) ) ;
#16678 = CARTESIAN_POINT ( 'NONE',  ( 0.000000000000000000, 0.000000000000000000, 0.000000000000000000 ) ) ;
#16679 = VERTEX_POINT ( 'NONE', #6478 ) ;
#16680 = CARTESIAN_POINT ( 'NONE',  ( -31.69597781366222122, 58.94165929845684815, 68.75000000000000000 ) ) ;
#16681 = EDGE_LOOP ( 'NONE', ( #18736, #8833, #1085, #1901 ) ) ;
#16682 = VERTEX_POINT ( 'NONE', #9712 ) ;
#16683 = CIRCLE ( 'NONE', #19552, 1.000000000000000888 ) ;
#16684 = EDGE_CURVE ( 'NONE', #10017, #21319, #6359, .T. ) ;
#16685 = AXIS2_PLACEMENT_3D ( 'NONE', #17219, #13851, #197 ) ;
#16686 = AXIS2_PLACEMENT_3D ( 'NONE', #5163, #11964, #4941 ) ;
#16687 = ORIENTED_EDGE ( 'NONE', *, *, #12144, .T. ) ;
#16688 = LINE ( 'NONE', #6764, #593 ) ;
#16689 = AXIS2_PLACEMENT_3D ( 'NONE', #9567, #12904, #13132 ) ;
#16690 = DIRECTION ( 'NONE',  ( 0.000000000000000000, 0.000000000000000000, 1.000000000000000000 ) ) ;
#16691 = AXIS2_PLACEMENT_3D ( 'NONE', #15818, #485, #7339 ) ;
#16692 = VERTEX_POINT ( 'NONE', #14729 ) ;
#16693 = PRESENTATION_STYLE_ASSIGNMENT (( #17930 ) ) ;
#16694 = EDGE_CURVE ( 'NONE', #19806, #6030, #6250, .T. ) ;
#16695 = LINE ( 'NONE', #5183, #2599 ) ;
#16696 = CARTESIAN_POINT ( 'NONE',  ( -15.95292532278785913, 50.11873716947361856, 13.87499999999999822 ) ) ;
#16697 = CARTESIAN_POINT ( 'NONE',  ( -29.17540678000427690, 6.499884319688664647, 7.500000000000000000 ) ) ;
#16698 = DIRECTION ( 'NONE',  ( -0.000000000000000000, 1.000000000000000000, -0.000000000000000000 ) ) ;
#16699 = AXIS2_PLACEMENT_3D ( 'NONE', #21146, #12384, #4347 ) ;
#16700 = ORIENTED_EDGE ( 'NONE', *, *, #18200, .T. ) ;
#16701 = VECTOR ( 'NONE', #18423, 1000.000000000000000 ) ;
#16702 = CIRCLE ( 'NONE', #5298, 0.04999999999999991257 ) ;
#16703 = VERTEX_POINT ( 'NONE', #13271 ) ;
#16704 = ORIENTED_EDGE ( 'NONE', *, *, #4716, .T. ) ;
#16705 = DIRECTION ( 'NONE',  ( 1.000000000000000000, 0.000000000000000000, -0.000000000000000000 ) ) ;
#16706 = DIRECTION ( 'NONE',  ( 0.000000000000000000, -0.000000000000000000, 1.000000000000000000 ) ) ;
#16707 = EDGE_LOOP ( 'NONE', ( #21119, #21692, #7161, #20021 ) ) ;
#16708 = CIRCLE ( 'NONE', #14216, 0.1000000000000028644 ) ;
#16709 = DIRECTION ( 'NONE',  ( 0.000000000000000000, 1.000000000000000000, 0.000000000000000000 ) ) ;
#16710 = VECTOR ( 'NONE', #14229, 1000.000000000000000 ) ;
#16711 = VECTOR ( 'NONE', #6084, 1000.000000000000000 ) ;
#16712 = EDGE_CURVE ( 'NONE', #18906, #17812, #5267, .T. ) ;
#16713 = ORIENTED_EDGE ( 'NONE', *, *, #2943, .F. ) ;
#16714 = CARTESIAN_POINT ( 'NONE',  ( 14.96174975910705918, 51.86873716947361856, 14.00000000000000000 ) ) ;
#16715 = LINE ( 'NONE', #2624, #19536 ) ;
#16716 = DIRECTION ( 'NONE',  ( 0.000000000000000000, 0.000000000000000000, 1.000000000000000000 ) ) ;
#16717 = AXIS2_PLACEMENT_3D ( 'NONE', #18762, #8707, #3436 ) ;
#16718 = AXIS2_PLACEMENT_3D ( 'NONE', #17108, #12052, #16982 ) ;
#16719 = CARTESIAN_POINT ( 'NONE',  ( -1.724728116533986721, 43.31054587065082728, 51.75876104995654003 ) ) ;
#16720 = ORIENTED_EDGE ( 'NONE', *, *, #9018, .F. ) ;
#16721 = DIRECTION ( 'NONE',  ( 0.000000000000000000, 0.000000000000000000, 1.000000000000000000 ) ) ;
#16722 = CYLINDRICAL_SURFACE ( 'NONE', #6426, 2.000000000000000000 ) ;
#16723 = EDGE_CURVE ( 'NONE', #3080, #13878, #7420, .T. ) ;
#16724 = EDGE_CURVE ( 'NONE', #1905, #20015, #20332, .T. ) ;
#16725 = AXIS2_PLACEMENT_3D ( 'NONE', #17223, #7502, #19025 ) ;
#16726 = FACE_OUTER_BOUND ( 'NONE', #6506, .T. ) ;
#16727 = DIRECTION ( 'NONE',  ( 0.000000000000000000, 0.000000000000000000, -1.000000000000000000 ) ) ;
#16728 = ORIENTED_EDGE ( 'NONE', *, *, #13726, .T. ) ;
#16729 = FACE_OUTER_BOUND ( 'NONE', #1131, .T. ) ;
#16730 = AXIS2_PLACEMENT_3D ( 'NONE', #1903, #8745, #15540 ) ;
#16731 = VECTOR ( 'NONE', #13504, 1000.000000000000000 ) ;
#16732 = ORIENTED_EDGE ( 'NONE', *, *, #3030, .F. ) ;
#16733 = DIRECTION ( 'NONE',  ( 0.000000000000000000, 0.000000000000000000, -1.000000000000000000 ) ) ;
#16734 = DIRECTION ( 'NONE',  ( -1.000000000000000000, -0.000000000000000000, 0.000000000000000000 ) ) ;
#16735 = ORIENTED_EDGE ( 'NONE', *, *, #14869, .T. ) ;
#16736 = ORIENTED_EDGE ( 'NONE', *, *, #7668, .T. ) ;
#16737 = ORIENTED_EDGE ( 'NONE', *, *, #21393, .F. ) ;
#16738 = CARTESIAN_POINT ( 'NONE',  ( 1.724728116533979838, 43.26054587065083012, 29.71679706732590631 ) ) ;
#16739 = FACE_OUTER_BOUND ( 'NONE', #19126, .T. ) ;
#16740 = DIRECTION ( 'NONE',  ( -0.000000000000000000, -0.000000000000000000, -1.000000000000000000 ) ) ;
#16741 = AXIS2_PLACEMENT_3D ( 'NONE', #20623, #12198, #8755 ) ;
#16742 = ORIENTED_EDGE ( 'NONE', *, *, #5634, .F. ) ;
#16743 = ADVANCED_FACE ( 'NONE', ( #1518 ), #6689, .F. ) ;
#16744 = CIRCLE ( 'NONE', #12092, 1.000000000000000888 ) ;
#16745 = ORIENTED_EDGE ( 'NONE', *, *, #19288, .T. ) ;
#16746 = DIRECTION ( 'NONE',  ( 1.000000000000000000, 0.000000000000000000, 0.000000000000000000 ) ) ;
#16747 = AXIS2_PLACEMENT_3D ( 'NONE', #21158, #8688, #22004 ) ;
#16748 = PLANE ( 'NONE',  #21376 ) ;
#16749 = DIRECTION ( 'NONE',  ( 0.000000000000000000, 0.000000000000000000, 1.000000000000000000 ) ) ;
#16750 = DIRECTION ( 'NONE',  ( 0.000000000000000000, 0.000000000000000000, -1.000000000000000000 ) ) ;
#16751 = DIRECTION ( 'NONE',  ( 1.000000000000000000, -0.000000000000000000, -0.000000000000000000 ) ) ;
#16752 = DIRECTION ( 'NONE',  ( -0.000000000000000000, 1.000000000000000000, -0.000000000000000000 ) ) ;
#16753 = EDGE_LOOP ( 'NONE', ( #2724, #20934, #16385, #11686 ) ) ;
#16754 = FACE_OUTER_BOUND ( 'NONE', #19404, .T. ) ;
#16755 = ADVANCED_FACE ( 'NONE', ( #5002 ), #16955, .T. ) ;
#16756 = EDGE_CURVE ( 'NONE', #21431, #3754, #8121, .T. ) ;
#16757 = CARTESIAN_POINT ( 'NONE',  ( -31.26086011588028057, 83.95073979834609190, 68.25000000000000000 ) ) ;
#16758 = DIRECTION ( 'NONE',  ( -0.000000000000000000, 1.000000000000000000, -0.000000000000000000 ) ) ;
#16759 = ORIENTED_EDGE ( 'NONE', *, *, #8826, .F. ) ;
#16760 = DIRECTION ( 'NONE',  ( -1.000000000000000000, 0.000000000000000000, 0.000000000000000000 ) ) ;
#16761 = ADVANCED_FACE ( 'NONE', ( #10040 ), #15163, .F. ) ;
#16762 = AXIS2_PLACEMENT_3D ( 'NONE', #1607, #9799, #18514 ) ;
#16763 = VERTEX_POINT ( 'NONE', #16847 ) ;
#16764 = DIRECTION ( 'NONE',  ( -0.000000000000000000, -1.000000000000000000, -0.000000000000000000 ) ) ;
#16765 = AXIS2_PLACEMENT_3D ( 'NONE', #12393, #17449, #12071 ) ;
#16766 = DIRECTION ( 'NONE',  ( -0.000000000000000000, -1.000000000000000000, -0.000000000000000000 ) ) ;
#16767 = ORIENTED_EDGE ( 'NONE', *, *, #15152, .T. ) ;
#16768 = ORIENTED_EDGE ( 'NONE', *, *, #9201, .T. ) ;
#16769 = LINE ( 'NONE', #6841, #10271 ) ;
#16770 = EDGE_CURVE ( 'NONE', #2469, #2743, #3117, .T. ) ;
#16771 = ORIENTED_EDGE ( 'NONE', *, *, #165, .T. ) ;
#16772 = CARTESIAN_POINT ( 'NONE',  ( -30.37540678000427619, 63.74634676501045050, 3.799999999999999822 ) ) ;
#16773 = VECTOR ( 'NONE', #16526, 1000.000000000000000 ) ;
#16774 = DIRECTION ( 'NONE',  ( 1.000000000000000000, 0.000000000000000000, 6.123233995736701941E-17 ) ) ;
#16775 = CIRCLE ( 'NONE', #19640, 0.9652499999999990532 ) ;
#16776 = CIRCLE ( 'NONE', #12819, 0.04999999999999991257 ) ;
#16777 = DIRECTION ( 'NONE',  ( -0.000000000000000000, -0.000000000000000000, -1.000000000000000000 ) ) ;
#16778 = CARTESIAN_POINT ( 'NONE',  ( -18.22752199202934520, -50.11873716947361856, 13.79999999999999893 ) ) ;
#16779 = ADVANCED_FACE ( 'NONE', ( #17284 ), #22011, .T. ) ;
#16780 = CARTESIAN_POINT ( 'NONE',  ( -25.37540678000427263, 68.44634676501046044, 7.200000000000000178 ) ) ;
#16781 = FACE_OUTER_BOUND ( 'NONE', #4304, .T. ) ;
#16782 = ADVANCED_FACE ( 'NONE', ( #6810 ), #5641, .F. ) ;
#16783 = DIRECTION ( 'NONE',  ( 0.000000000000000000, 0.000000000000000000, 1.000000000000000000 ) ) ;
#16784 = CARTESIAN_POINT ( 'NONE',  ( -14.98564789012718101, -51.95085597973990588, 13.85527924978055481 ) ) ;
#16785 = LINE ( 'NONE', #14878, #1597 ) ;
#16786 = AXIS2_PLACEMENT_3D ( 'NONE', #6223, #14592, #1059 ) ;
#16787 = ORIENTED_EDGE ( 'NONE', *, *, #21778, .T. ) ;
#16788 = DIRECTION ( 'NONE',  ( -0.000000000000000000, 0.000000000000000000, 1.000000000000000000 ) ) ;
#16789 = VERTEX_POINT ( 'NONE', #164 ) ;
#16790 = LINE ( 'NONE', #6748, #11307 ) ;
#16791 = AXIS2_PLACEMENT_3D ( 'NONE', #584, #7325, #9101 ) ;
#16792 = PRODUCT_DEFINITION_SHAPE ( 'NONE', 'NONE',  #22167 ) ;
#16793 = ORIENTED_EDGE ( 'NONE', *, *, #3129, .F. ) ;
#16794 = ORIENTED_EDGE ( 'NONE', *, *, #9180, .F. ) ;
#16795 = CARTESIAN_POINT ( 'NONE',  ( -34.40000000000001279, -84.70000000000001705, 80.00000000000000000 ) ) ;
#16796 = ORIENTED_EDGE ( 'NONE', *, *, #1784, .F. ) ;
#16797 = EDGE_LOOP ( 'NONE', ( #5513, #21136, #1521, #1080 ) ) ;
#16798 = EDGE_CURVE ( 'NONE', #12793, #170, #10142, .T. ) ;
#16799 = ORIENTED_EDGE ( 'NONE', *, *, #14245, .T. ) ;
#16800 = EDGE_CURVE ( 'NONE', #7338, #15871, #13113, .T. ) ;
#16801 = ORIENTED_EDGE ( 'NONE', *, *, #6432, .F. ) ;
#16802 = TOROIDAL_SURFACE ( 'NONE', #11438, 0.05000000000000000278, 0.05000000000000000278 ) ;
#16803 = LINE ( 'NONE', #15119, #12693 ) ;
#16804 = DIRECTION ( 'NONE',  ( -0.7193398003386523021, 0.000000000000000000, 0.6946583704589960329 ) ) ;
#16805 = AXIS2_PLACEMENT_3D ( 'NONE', #6185, #9412, #13081 ) ;
#16806 = DIRECTION ( 'NONE',  ( 0.000000000000000000, 1.000000000000000000, 0.000000000000000000 ) ) ;
#16807 = ORIENTED_EDGE ( 'NONE', *, *, #21601, .F. ) ;
#16808 = DIRECTION ( 'NONE',  ( 0.000000000000000000, 0.000000000000000000, 1.000000000000000000 ) ) ;
#16809 = DIRECTION ( 'NONE',  ( -1.000000000000000000, 0.000000000000000000, 0.000000000000000000 ) ) ;
#16810 = CYLINDRICAL_SURFACE ( 'NONE', #12547, 0.3000000000000016542 ) ;
#16811 = DIRECTION ( 'NONE',  ( 0.000000000000000000, 0.000000000000000000, 1.000000000000000000 ) ) ;
#16812 = DIRECTION ( 'NONE',  ( -0.000000000000000000, 1.000000000000000000, -0.000000000000000000 ) ) ;
#16813 = VERTEX_POINT ( 'NONE', #15280 ) ;
#16814 = VERTEX_POINT ( 'NONE', #22138 ) ;
#16815 = ORIENTED_EDGE ( 'NONE', *, *, #13550, .T. ) ;
#16816 = CARTESIAN_POINT ( 'NONE',  ( 1.724728116533979616, 42.36054587065083155, 29.76679706732590702 ) ) ;
#16817 = CARTESIAN_POINT ( 'NONE',  ( 1.724728116533979838, 42.36054587065083155, 49.66679706732590915 ) ) ;
#16818 = ORIENTED_EDGE ( 'NONE', *, *, #14674, .T. ) ;
#16819 = VECTOR ( 'NONE', #11295, 1000.000000000000000 ) ;
#16820 = LINE ( 'NONE', #11558, #19494 ) ;
#16821 = ORIENTED_EDGE ( 'NONE', *, *, #18483, .T. ) ;
#16822 = CARTESIAN_POINT ( 'NONE',  ( -34.39999999999999858, -84.70000000000001705, 0.6000000000000033085 ) ) ;
#16823 = ADVANCED_FACE ( 'NONE', ( #5225 ), #13609, .F. ) ;
#16824 = LINE ( 'NONE', #5201, #17387 ) ;
#16825 = VECTOR ( 'NONE', #16727, 1000.000000000000000 ) ;
#16826 = CYLINDRICAL_SURFACE ( 'NONE', #22061, 0.2500000000000002220 ) ;
#16827 = AXIS2_PLACEMENT_3D ( 'NONE', #7448, #7229, #17610 ) ;
#16828 = DIRECTION ( 'NONE',  ( 0.000000000000000000, -1.000000000000000000, 0.000000000000000000 ) ) ;
#16829 = ORIENTED_EDGE ( 'NONE', *, *, #8985, .F. ) ;
#16830 = CARTESIAN_POINT ( 'NONE',  ( 23.32398829872514057, 2.157133568460765538, 13.50000000000000000 ) ) ;
#16831 = DIRECTION ( 'NONE',  ( 0.000000000000000000, -1.000000000000000000, 0.000000000000000000 ) ) ;
#16832 = VECTOR ( 'NONE', #7025, 1000.000000000000000 ) ;
#16833 = DIRECTION ( 'NONE',  ( -0.000000000000000000, 1.000000000000000000, -0.000000000000000000 ) ) ;
#16834 = DIRECTION ( 'NONE',  ( -1.000000000000000000, 0.000000000000000000, 0.000000000000000000 ) ) ;
#16835 = LINE ( 'NONE', #15154, #4379 ) ;
#16836 = EDGE_LOOP ( 'NONE', ( #10192, #17135 ) ) ;
#16837 = DIRECTION ( 'NONE',  ( 0.000000000000000000, 1.000000000000000000, 0.000000000000000000 ) ) ;
#16838 = LINE ( 'NONE', #14750, #10346 ) ;
#16839 = ORIENTED_EDGE ( 'NONE', *, *, #7127, .F. ) ;
#16840 = CARTESIAN_POINT ( 'NONE',  ( -9.141460742840918030, 33.93424481021354921, 68.00000000000000000 ) ) ;
#16841 = CIRCLE ( 'NONE', #14330, 0.2999999999999999334 ) ;
#16842 = DIRECTION ( 'NONE',  ( 0.000000000000000000, 0.000000000000000000, 1.000000000000000000 ) ) ;
#16843 = EDGE_CURVE ( 'NONE', #12408, #5130, #13815, .T. ) ;
#16844 = ORIENTED_EDGE ( 'NONE', *, *, #18728, .F. ) ;
#16845 = VERTEX_POINT ( 'NONE', #8793 ) ;
#16846 = ORIENTED_EDGE ( 'NONE', *, *, #17253, .F. ) ;
#16847 = CARTESIAN_POINT ( 'NONE',  ( 4.127054932750481520, -33.93424481021354921, 68.50000000000000000 ) ) ;
#16848 = AXIS2_PLACEMENT_3D ( 'NONE', #21428, #12889, #19969 ) ;
#16849 = DIRECTION ( 'NONE',  ( 0.000000000000000000, -1.000000000000000000, 0.000000000000000000 ) ) ;
#16850 = CIRCLE ( 'NONE', #8290, 0.5000000000000004441 ) ;
#16851 =( BOUNDED_CURVE ( )  B_SPLINE_CURVE ( 3, ( #9280, #323, #2117, #5603 ),
 .UNSPECIFIED., .F., .T. ) 
 B_SPLINE_CURVE_WITH_KNOTS ( ( 4, 4 ),
 ( 0.000000000000000000, 1.570796326794896558 ),
 .UNSPECIFIED. ) 
 CURVE ( )  GEOMETRIC_REPRESENTATION_ITEM ( )  RATIONAL_B_SPLINE_CURVE ( ( 1.000000000000000000, 0.8047378541243649375, 0.8047378541243649375, 1.000000000000000000 ) ) 
 REPRESENTATION_ITEM ( '' )  );
#16852 = ORIENTED_EDGE ( 'NONE', *, *, #18918, .T. ) ;
#16853 = ADVANCED_FACE ( 'NONE', ( #15597 ), #16675, .T. ) ;
#16854 = VERTEX_POINT ( 'NONE', #276 ) ;
#16855 = EDGE_CURVE ( 'NONE', #1525, #14178, #19546, .T. ) ;
#16856 = ORIENTED_EDGE ( 'NONE', *, *, #12806, .F. ) ;
#16857 = DIRECTION ( 'NONE',  ( -3.052134192567367925E-16, -1.000000000000000000, 0.000000000000000000 ) ) ;
#16858 = VERTEX_POINT ( 'NONE', #17393 ) ;
#16859 = DIRECTION ( 'NONE',  ( 0.000000000000000000, 1.000000000000000000, 0.000000000000000000 ) ) ;
#16860 = CARTESIAN_POINT ( 'NONE',  ( -1.724728116533986721, 42.36054587065083155, 43.80876104995653719 ) ) ;
#16861 = CIRCLE ( 'NONE', #5804, 0.2500000000000002220 ) ;
#16862 = FACE_OUTER_BOUND ( 'NONE', #7878, .T. ) ;
#16863 = CARTESIAN_POINT ( 'NONE',  ( -29.50000000000002132, -2.473451120191013430, 0.2999999999999947153 ) ) ;
#16864 = DIRECTION ( 'NONE',  ( 1.000000000000000000, -0.000000000000000000, -0.000000000000000000 ) ) ;
#16865 = AXIS2_PLACEMENT_3D ( 'NONE', #21518, #9308, #7740 ) ;
#16866 = AXIS2_PLACEMENT_3D ( 'NONE', #2112, #7275, #5599 ) ;
#16867 = CARTESIAN_POINT ( 'NONE',  ( 1.724728116533979838, 43.26054587065083012, 45.71679706732590631 ) ) ;
#16868 = DIRECTION ( 'NONE',  ( 1.000000000000000000, 0.000000000000000000, 0.000000000000000000 ) ) ;
#16869 = ORIENTED_EDGE ( 'NONE', *, *, #6994, .F. ) ;
#16870 = CARTESIAN_POINT ( 'NONE',  ( 30.50000000000000000, 70.29999999999999716, 1.500000000000003997 ) ) ;
#16871 = EDGE_CURVE ( 'NONE', #5205, #2890, #4082, .T. ) ;
#16872 = CYLINDRICAL_SURFACE ( 'NONE', #15560, 0.3000000000000016542 ) ;
#16873 = VERTEX_POINT ( 'NONE', #9337 ) ;
#16874 = DIRECTION ( 'NONE',  ( 1.000000000000000000, -0.000000000000000000, -0.000000000000000000 ) ) ;
#16875 = PLANE ( 'NONE',  #7101 ) ;
#16876 = ORIENTED_EDGE ( 'NONE', *, *, #16895, .T. ) ;
#16877 = EDGE_LOOP ( 'NONE', ( #1928, #12167, #14481, #7234 ) ) ;
#16878 = CARTESIAN_POINT ( 'NONE',  ( 25.37540678000427263, -63.74634676501045050, 7.799999999999999822 ) ) ;
#16879 = EDGE_CURVE ( 'NONE', #13276, #21191, #16142, .T. ) ;
#16880 = CIRCLE ( 'NONE', #5819, 0.2999999999999999889 ) ;
#16881 = EDGE_CURVE ( 'NONE', #1455, #252, #2300, .T. ) ;
#16882 = COLOUR_RGB ( '', 0.40784314, 0.44705882, 0.49803922) ;
#16883 = EDGE_CURVE ( 'NONE', #10410, #19345, #15713, .T. ) ;
#16884 = EDGE_LOOP ( 'NONE', ( #19896, #6973, #11044, #16829 ) ) ;
#16885 = EDGE_CURVE ( 'NONE', #1148, #21866, #19392, .T. ) ;
#16886 = CARTESIAN_POINT ( 'NONE',  ( -29.17540678000427690, -63.74634676501045050, 7.799999999999999822 ) ) ;
#16887 = VERTEX_POINT ( 'NONE', #19514 ) ;
#16888 = CARTESIAN_POINT ( 'NONE',  ( -27.37540678000427619, 7.754037881813018962E-15, 42.50000000000000000 ) ) ;
#16889 = DIRECTION ( 'NONE',  ( 0.000000000000000000, -1.000000000000000000, 0.000000000000000000 ) ) ;
#16890 = CONICAL_SURFACE ( 'NONE', #19043, 0.9652499999999990532, 0.06981317007976590994 ) ;
#16891 = CARTESIAN_POINT ( 'NONE',  ( -4.127054932750482408, 32.93424481021354921, 68.00000000000000000 ) ) ;
#16892 = DIRECTION ( 'NONE',  ( 2.107255972849994642E-16, -0.000000000000000000, 1.000000000000000000 ) ) ;
#16893 = LINE ( 'NONE', #18922, #13556 ) ;
#16894 = CARTESIAN_POINT ( 'NONE',  ( 0.000000000000000000, 43.31054587065082728, 24.00000000000000000 ) ) ;
#16895 = EDGE_CURVE ( 'NONE', #17181, #3127, #21215, .T. ) ;
#16896 = CARTESIAN_POINT ( 'NONE',  ( -25.37540678000427263, 68.74634676501045760, 7.500000000000000000 ) ) ;
#16897 = CARTESIAN_POINT ( 'NONE',  ( -15.07123959906592248, -52.06981400416638905, 13.87294810141926149 ) ) ;
#16898 = CARTESIAN_POINT ( 'NONE',  ( -10.13407133124522908, 43.00645089659918341, 69.94509975324523054 ) ) ;
#16899 = ORIENTED_EDGE ( 'NONE', *, *, #19837, .F. ) ;
#16900 = DIRECTION ( 'NONE',  ( 0.000000000000000000, 1.000000000000000000, 0.000000000000000000 ) ) ;
#16901 = EDGE_LOOP ( 'NONE', ( #6255, #7015, #19631, #3304 ) ) ;
#16902 = DIRECTION ( 'NONE',  ( 0.000000000000000000, -1.000000000000000000, 0.000000000000000000 ) ) ;
#16903 = DIRECTION ( 'NONE',  ( 0.000000000000000000, 0.000000000000000000, 1.000000000000000000 ) ) ;
#16904 = ORIENTED_EDGE ( 'NONE', *, *, #16770, .T. ) ;
#16905 = ORIENTED_EDGE ( 'NONE', *, *, #21624, .T. ) ;
#16906 = CARTESIAN_POINT ( 'NONE',  ( 0.000000000000000000, -38.74634676501045760, 13.79999999999999893 ) ) ;
#16907 = ORIENTED_EDGE ( 'NONE', *, *, #3375, .F. ) ;
#16908 = EDGE_CURVE ( 'NONE', #11436, #2833, #14199, .T. ) ;
#16909 = EDGE_CURVE ( 'NONE', #2503, #3013, #21366, .T. ) ;
#16910 = ORIENTED_EDGE ( 'NONE', *, *, #17052, .F. ) ;
#16911 = PRODUCT_DEFINITION_CONTEXT ( 'detailed design', #10013, 'design' ) ;
#16912 = ORIENTED_EDGE ( 'NONE', *, *, #1930, .F. ) ;
#16913 = CARTESIAN_POINT ( 'NONE',  ( -26.37540678000427619, 10.94079601157914539, 13.79999999999999893 ) ) ;
#16914 = B_SPLINE_CURVE_WITH_KNOTS ( 'NONE', 3,
 ( #20947, #5519, #17475, #2251, #9083, #21075, #15884, #9192 ),
 .UNSPECIFIED., .F., .F.,
 ( 4, 2, 2, 4 ),
 ( -3.470042892451968281E-06, 0.0002769752510348927397, 0.0004171978979985645165, 0.0005574205449622362391 ),
 .UNSPECIFIED. ) ;
#16915 = CARTESIAN_POINT ( 'NONE',  ( 14.96174975910705918, -51.76873716947361004, 13.79999999999999716 ) ) ;
#16916 = DIRECTION ( 'NONE',  ( -0.000000000000000000, 1.000000000000000000, 0.000000000000000000 ) ) ;
#16917 = ORIENTED_EDGE ( 'NONE', *, *, #16185, .T. ) ;
#16918 = DIRECTION ( 'NONE',  ( -0.000000000000000000, -0.000000000000000000, -1.000000000000000000 ) ) ;
#16919 = CARTESIAN_POINT ( 'NONE',  ( -35.00000000000000000, 84.70000000000001705, 0.000000000000000000 ) ) ;
#16920 = LINE ( 'NONE', #13570, #21868 ) ;
#16921 = CARTESIAN_POINT ( 'NONE',  ( 30.07540678000427548, -6.000000000000000000, 7.200000000000000178 ) ) ;
#16922 = ADVANCED_FACE ( 'NONE', ( #5784 ), #5678, .T. ) ;
#16923 = DIRECTION ( 'NONE',  ( 1.000000000000000000, 0.000000000000000000, 0.000000000000000000 ) ) ;
#16924 = ORIENTED_EDGE ( 'NONE', *, *, #14138, .T. ) ;
#16925 = ORIENTED_EDGE ( 'NONE', *, *, #13100, .T. ) ;
#16926 = ORIENTED_EDGE ( 'NONE', *, *, #14757, .F. ) ;
#16927 = CYLINDRICAL_SURFACE ( 'NONE', #6376, 4.193574995607837863 ) ;
#16928 = ORIENTED_EDGE ( 'NONE', *, *, #2043, .T. ) ;
#16929 = B_SPLINE_CURVE_WITH_KNOTS ( 'NONE', 3,
 ( #2146, #19054, #3507, #3954, #10445, #8661, #3722, #15679, #238, #10340, #8874, #12426, #1822, #12204 ),
 .UNSPECIFIED., .F., .F.,
 ( 4, 2, 2, 2, 2, 2, 4 ),
 ( 0.000000000000000000, 0.0006835338044177905739, 0.001025300706626683855, 0.001196184157731130333, 0.001281625883283352705, 0.001324346746059462806, 0.001367067608835572691 ),
 .UNSPECIFIED. ) ;
#16930 = CARTESIAN_POINT ( 'NONE',  ( 14.96243083687292952, -51.84435441965536739, 13.82657707279502546 ) ) ;
#16931 = ADVANCED_FACE ( 'NONE', ( #19307 ), #5450, .T. ) ;
#16932 = VECTOR ( 'NONE', #1120, 1000.000000000000000 ) ;
#16933 = ORIENTED_EDGE ( 'NONE', *, *, #5639, .F. ) ;
#16934 = CARTESIAN_POINT ( 'NONE',  ( 25.37540678000427263, -63.74634676501045050, 7.200000000000000178 ) ) ;
#16935 = AXIS2_PLACEMENT_3D ( 'NONE', #20200, #2974, #8238 ) ;
#16936 = DIRECTION ( 'NONE',  ( 0.000000000000000000, 0.000000000000000000, 1.000000000000000000 ) ) ;
#16937 = CARTESIAN_POINT ( 'NONE',  ( -14.96174975910705207, -51.61873716947361856, 14.00000000000000000 ) ) ;
#16938 = ORIENTED_EDGE ( 'NONE', *, *, #2093, .T. ) ;
#16939 = CARTESIAN_POINT ( 'NONE',  ( 1.774728116533979438, 42.36054587065083155, 43.80876104995653719 ) ) ;
#16940 = CARTESIAN_POINT ( 'NONE',  ( -8.149501154770138811, 41.92645089659918511, 70.88527860057354246 ) ) ;
#16941 = DIRECTION ( 'NONE',  ( 0.2309407893632113573, -0.9729678061520313781, 0.000000000000000000 ) ) ;
#16942 = CARTESIAN_POINT ( 'NONE',  ( 25.37540678000429040, -36.74634676501047181, 13.79999999999999893 ) ) ;
#16943 = CARTESIAN_POINT ( 'NONE',  ( 34.39999999999998437, -84.70000000000001705, 79.39999999999999147 ) ) ;
#16944 = ORIENTED_EDGE ( 'NONE', *, *, #14319, .F. ) ;
#16945 = CARTESIAN_POINT ( 'NONE',  ( -26.63662752439704917, -3.061616997868386099E-16, 3.500000000000000000 ) ) ;
#16946 = EDGE_CURVE ( 'NONE', #19232, #9803, #14258, .T. ) ;
#16947 = ORIENTED_EDGE ( 'NONE', *, *, #20385, .T. ) ;
#16948 = DIRECTION ( 'NONE',  ( -1.224646799147353207E-16, -0.000000000000000000, -1.000000000000000000 ) ) ;
#16949 = DIRECTION ( 'NONE',  ( 0.000000000000000000, 0.000000000000000000, -1.000000000000000000 ) ) ;
#16950 = EDGE_CURVE ( 'NONE', #17432, #5083, #5884, .T. ) ;
#16951 = ORIENTED_EDGE ( 'NONE', *, *, #12542, .T. ) ;
#16952 = ORIENTED_EDGE ( 'NONE', *, *, #11850, .T. ) ;
#16953 = AXIS2_PLACEMENT_3D ( 'NONE', #15029, #11655, #1484 ) ;
#16954 = EDGE_LOOP ( 'NONE', ( #843, #18480, #20984, #21115 ) ) ;
#16955 = PLANE ( 'NONE',  #8836 ) ;
#16956 = CARTESIAN_POINT ( 'NONE',  ( -1.724728116533986721, 43.31054587065082728, 27.70876104995653577 ) ) ;
#16957 = FACE_OUTER_BOUND ( 'NONE', #12520, .T. ) ;
#16958 = ORIENTED_EDGE ( 'NONE', *, *, #328, .T. ) ;
#16959 = CARTESIAN_POINT ( 'NONE',  ( -1.724728116533986721, 43.26054587065083012, 47.70876104995654288 ) ) ;
#16960 = ORIENTED_EDGE ( 'NONE', *, *, #17174, .T. ) ;
#16961 = ORIENTED_EDGE ( 'NONE', *, *, #14754, .F. ) ;
#16962 = DIRECTION ( 'NONE',  ( 1.000000000000000000, 0.000000000000000000, 0.000000000000000000 ) ) ;
#16963 = ORIENTED_EDGE ( 'NONE', *, *, #18247, .T. ) ;
#16964 = DIRECTION ( 'NONE',  ( 0.000000000000000000, -1.000000000000000000, 0.000000000000000000 ) ) ;
#16965 = DIRECTION ( 'NONE',  ( 0.000000000000000000, -1.000000000000000000, 0.000000000000000000 ) ) ;
#16966 = EDGE_CURVE ( 'NONE', #1026, #20751, #18485, .T. ) ;
#16967 = AXIS2_PLACEMENT_3D ( 'NONE', #18249, #6290, #6743 ) ;
#16968 = CARTESIAN_POINT ( 'NONE',  ( 1.724728116533979616, 42.36054587065083155, 39.80876104995653719 ) ) ;
#16969 = CIRCLE ( 'NONE', #7337, 0.05000000000000143219 ) ;
#16970 = DIRECTION ( 'NONE',  ( 1.000000000000000000, 0.000000000000000000, 0.000000000000000000 ) ) ;
#16971 = VERTEX_POINT ( 'NONE', #3876 ) ;
#16972 = CARTESIAN_POINT ( 'NONE',  ( 23.02398829872513630, 2.211005466174524425, 13.25091654438544353 ) ) ;
#16973 = DIRECTION ( 'NONE',  ( 1.000000000000000000, 0.000000000000000000, 0.000000000000000000 ) ) ;
#16974 = CARTESIAN_POINT ( 'NONE',  ( -1.824728116533986810, 42.36054587065083155, 51.80876104995653719 ) ) ;
#16975 = DIRECTION ( 'NONE',  ( 1.000000000000000000, 0.000000000000000000, -0.000000000000000000 ) ) ;
#16976 = ORIENTED_EDGE ( 'NONE', *, *, #18025, .F. ) ;
#16977 = CARTESIAN_POINT ( 'NONE',  ( 14.71174975910706451, 50.19799549595485644, 68.50000000000000000 ) ) ;
#16978 = EDGE_CURVE ( 'NONE', #3289, #5001, #2180, .T. ) ;
#16979 = CARTESIAN_POINT ( 'NONE',  ( -1.724728116533986721, 43.31054587065082728, 45.76679706732590347 ) ) ;
#16980 = ORIENTED_EDGE ( 'NONE', *, *, #16724, .F. ) ;
#16981 = DIRECTION ( 'NONE',  ( -0.000000000000000000, -0.000000000000000000, -1.000000000000000000 ) ) ;
#16982 = DIRECTION ( 'NONE',  ( -1.000000000000000000, 0.000000000000000000, 0.000000000000000000 ) ) ;
#16983 = AXIS2_PLACEMENT_3D ( 'NONE', #18980, #15706, #12332 ) ;
#16984 = VERTEX_POINT ( 'NONE', #9016 ) ;
#16985 = AXIS2_PLACEMENT_3D ( 'NONE', #3570, #13515, #20358 ) ;
#16986 = DIRECTION ( 'NONE',  ( -2.388292521039847891E-16, 0.000000000000000000, -1.000000000000000000 ) ) ;
#16987 = ORIENTED_EDGE ( 'NONE', *, *, #3325, .F. ) ;
#16988 = EDGE_CURVE ( 'NONE', #12192, #14287, #17074, .T. ) ;
#16989 = EDGE_LOOP ( 'NONE', ( #20536, #14017, #13674, #2637 ) ) ;
#16990 = DIRECTION ( 'NONE',  ( -0.000000000000000000, 0.000000000000000000, 1.000000000000000000 ) ) ;
#16991 = AXIS2_PLACEMENT_3D ( 'NONE', #5926, #13184, #9620 ) ;
#16992 = FACE_OUTER_BOUND ( 'NONE', #15068, .T. ) ;
#16993 = DIRECTION ( 'NONE',  ( 1.000000000000000000, 0.000000000000000000, -0.000000000000000000 ) ) ;
#16994 = DIRECTION ( 'NONE',  ( -2.128201741475310638E-16, -0.4461977533474360547, -0.8949343913984424415 ) ) ;
#16995 = FACE_OUTER_BOUND ( 'NONE', #16514, .T. ) ;
#16996 = VECTOR ( 'NONE', #17272, 1000.000000000000000 ) ;
#16997 = VECTOR ( 'NONE', #6459, 1000.000000000000000 ) ;
#16998 = CARTESIAN_POINT ( 'NONE',  ( 14.96174975910705918, 51.61873716947361856, 14.00000000000000000 ) ) ;
#16999 = ADVANCED_FACE ( 'NONE', ( #14134 ), #20989, .F. ) ;
#17000 = ADVANCED_FACE ( 'NONE', ( #9785 ), #17782, .T. ) ;
#17001 = DIRECTION ( 'NONE',  ( 1.000000000000000000, 0.000000000000000000, 0.000000000000000000 ) ) ;
#17002 = EDGE_CURVE ( 'NONE', #2728, #8181, #2044, .T. ) ;
#17003 = CARTESIAN_POINT ( 'NONE',  ( -14.96174975910705207, -51.76873716947361714, 13.50000000000000000 ) ) ;
#17004 = DIRECTION ( 'NONE',  ( 0.000000000000000000, 0.000000000000000000, -1.000000000000000000 ) ) ;
#17005 = DIRECTION ( 'NONE',  ( -1.000000000000000000, 0.000000000000000000, 0.000000000000000000 ) ) ;
#17006 = CARTESIAN_POINT ( 'NONE',  ( -30.37540678000427619, -63.74634676501045050, 3.799999999999999822 ) ) ;
#17007 = CIRCLE ( 'NONE', #13785, 4.699999999999999289 ) ;
#17008 = AXIS2_PLACEMENT_3D ( 'NONE', #9898, #3519, #20304 ) ;
#17009 = ORIENTED_EDGE ( 'NONE', *, *, #13520, .T. ) ;
#17010 = AXIS2_PLACEMENT_3D ( 'NONE', #15725, #17955, #395 ) ;
#17011 = ORIENTED_EDGE ( 'NONE', *, *, #21285, .F. ) ;
#17012 = CARTESIAN_POINT ( 'NONE',  ( -35.00000000000001421, 84.70000000000001705, 80.00000000000000000 ) ) ;
#17013 = DIRECTION ( 'NONE',  ( 0.000000000000000000, 0.000000000000000000, -1.000000000000000000 ) ) ;
#17014 = ORIENTED_EDGE ( 'NONE', *, *, #17867, .T. ) ;
#17015 = CIRCLE ( 'NONE', #14854, 0.2999999999999947153 ) ;
#17016 = EDGE_CURVE ( 'NONE', #15626, #15586, #4569, .T. ) ;
#17017 = ORIENTED_EDGE ( 'NONE', *, *, #21586, .T. ) ;
#17018 = ORIENTED_EDGE ( 'NONE', *, *, #6362, .T. ) ;
#17019 = CARTESIAN_POINT ( 'NONE',  ( -23.61959064016851073, 45.26242829375641463, 13.74999999999999822 ) ) ;
#17020 = FACE_OUTER_BOUND ( 'NONE', #2345, .T. ) ;
#17021 = CARTESIAN_POINT ( 'NONE',  ( -9.141460742840918030, -33.93424481021354921, 68.00000000000000000 ) ) ;
#17022 = CIRCLE ( 'NONE', #19903, 0.04999999999999991257 ) ;
#17023 = VECTOR ( 'NONE', #6793, 1000.000000000000000 ) ;
#17024 = CIRCLE ( 'NONE', #7395, 0.1000000000000028644 ) ;
#17025 = DIRECTION ( 'NONE',  ( 1.000000000000000000, 0.000000000000000000, 0.000000000000000000 ) ) ;
#17026 = VECTOR ( 'NONE', #20255, 1000.000000000000000 ) ;
#17027 = CARTESIAN_POINT ( 'NONE',  ( -32.23382792203230451, 83.71979900898288918, 13.75000000000000000 ) ) ;
#17028 = ADVANCED_FACE ( 'NONE', ( #14586 ), #9684, .T. ) ;
#17029 = DIRECTION ( 'NONE',  ( 0.000000000000000000, 0.000000000000000000, 1.000000000000000000 ) ) ;
#17030 = ADVANCED_FACE ( 'NONE', ( #14915 ), #19746, .F. ) ;
#17031 = DIRECTION ( 'NONE',  ( -0.000000000000000000, 0.000000000000000000, 1.000000000000000000 ) ) ;
#17032 = CARTESIAN_POINT ( 'NONE',  ( 1.774728116533979438, 43.31054587065082728, 51.80876104995653719 ) ) ;
#17033 = DIRECTION ( 'NONE',  ( -1.000000000000000000, 0.000000000000000000, 0.000000000000000000 ) ) ;
#17034 = CIRCLE ( 'NONE', #3821, 0.05000000000000143219 ) ;
#17035 = EDGE_CURVE ( 'NONE', #12623, #12088, #10637, .T. ) ;
#17036 = VERTEX_POINT ( 'NONE', #11117 ) ;
#17037 = LINE ( 'NONE', #1588, #76 ) ;
#17038 = ORIENTED_EDGE ( 'NONE', *, *, #4424, .T. ) ;
#17039 = VERTEX_POINT ( 'NONE', #7998 ) ;
#17040 = ORIENTED_EDGE ( 'NONE', *, *, #7344, .T. ) ;
#17041 = CARTESIAN_POINT ( 'NONE',  ( 30.07540678000427548, -6.000000000000000000, 7.500000000000000000 ) ) ;
#17042 = CARTESIAN_POINT ( 'NONE',  ( -1.824728116533986810, 42.36054587065083155, 51.75876104995654003 ) ) ;
#17043 = ORIENTED_EDGE ( 'NONE', *, *, #11090, .T. ) ;
#17044 = CIRCLE ( 'NONE', #18842, 0.2999999999999999334 ) ;
#17045 = AXIS2_PLACEMENT_3D ( 'NONE', #11527, #1346, #4821 ) ;
#17046 = CYLINDRICAL_SURFACE ( 'NONE', #10235, 0.2999999999999999334 ) ;
#17047 = EDGE_CURVE ( 'NONE', #11031, #11974, #8156, .T. ) ;
#17048 = AXIS2_PLACEMENT_3D ( 'NONE', #14463, #7783, #9564 ) ;
#17049 = ORIENTED_EDGE ( 'NONE', *, *, #5541, .F. ) ;
#17050 = CARTESIAN_POINT ( 'NONE',  ( -9.641460742840918030, -32.11873716947361856, 109.6002446535588319 ) ) ;
#17051 = VECTOR ( 'NONE', #4556, 1000.000000000000000 ) ;
#17052 = EDGE_CURVE ( 'NONE', #20269, #14744, #7781, .T. ) ;
#17053 = CARTESIAN_POINT ( 'NONE',  ( -30.79999999999999361, -123.9599366953518711, 1.199999999999999734 ) ) ;
#17054 = DIRECTION ( 'NONE',  ( 0.000000000000000000, -0.000000000000000000, -1.000000000000000000 ) ) ;
#17055 = ORIENTED_EDGE ( 'NONE', *, *, #10824, .T. ) ;
#17056 = DIRECTION ( 'NONE',  ( 0.000000000000000000, 0.000000000000000000, 1.000000000000000000 ) ) ;
#17057 = DIRECTION ( 'NONE',  ( -2.832483164223434527E-16, 1.000000000000000000, 0.000000000000000000 ) ) ;
#17058 = CARTESIAN_POINT ( 'NONE',  ( 1.774728116533979660, 43.31054587065082728, 29.66679706732590560 ) ) ;
#17059 = DIRECTION ( 'NONE',  ( 0.000000000000000000, 0.000000000000000000, 1.000000000000000000 ) ) ;
#17060 = CARTESIAN_POINT ( 'NONE',  ( 28.87540678000427619, 63.74634676501045050, 7.799999999999999822 ) ) ;
#17061 = ORIENTED_EDGE ( 'NONE', *, *, #748, .F. ) ;
#17062 = CIRCLE ( 'NONE', #19570, 6.800000000000000711 ) ;
#17063 = VECTOR ( 'NONE', #19677, 1000.000000000000000 ) ;
#17064 = AXIS2_PLACEMENT_3D ( 'NONE', #5835, #12617, #19457 ) ;
#17065 = DIRECTION ( 'NONE',  ( 0.000000000000000000, -0.000000000000000000, 1.000000000000000000 ) ) ;
#17066 = EDGE_CURVE ( 'NONE', #18311, #13976, #12436, .T. ) ;
#17067 = EDGE_LOOP ( 'NONE', ( #15157, #1282, #21907, #7921 ) ) ;
#17068 = DIRECTION ( 'NONE',  ( 0.000000000000000000, -1.000000000000000000, 0.000000000000000000 ) ) ;
#17069 = DIRECTION ( 'NONE',  ( -0.000000000000000000, -1.000000000000000000, -0.000000000000000000 ) ) ;
#17070 = AXIS2_PLACEMENT_3D ( 'NONE', #15821, #10808, #12573 ) ;
#17071 = DIRECTION ( 'NONE',  ( 0.000000000000000000, 1.000000000000000000, 0.000000000000000000 ) ) ;
#17072 = ORIENTED_EDGE ( 'NONE', *, *, #16660, .T. ) ;
#17073 = ORIENTED_EDGE ( 'NONE', *, *, #21093, .F. ) ;
#17074 = CIRCLE ( 'NONE', #16691, 3.017785046117004377 ) ;
#17075 = ORIENTED_EDGE ( 'NONE', *, *, #13630, .T. ) ;
#17076 = DIRECTION ( 'NONE',  ( 1.000000000000000000, 0.000000000000000000, 0.000000000000000000 ) ) ;
#17077 = CARTESIAN_POINT ( 'NONE',  ( -1.724728116533986721, 42.31054587065082728, 53.66679706732590915 ) ) ;
#17078 = AXIS2_PLACEMENT_3D ( 'NONE', #13322, #16559, #8081 ) ;
#17079 = CARTESIAN_POINT ( 'NONE',  ( 8.641460742840918030, -32.93424481021354921, 42.50000000000000000 ) ) ;
#17080 = ORIENTED_EDGE ( 'NONE', *, *, #16381, .F. ) ;
#17081 = DIRECTION ( 'NONE',  ( 1.000000000000000000, 0.000000000000000000, 0.000000000000000000 ) ) ;
#17082 = EDGE_LOOP ( 'NONE', ( #2622, #6097, #5514, #10858 ) ) ;
#17083 = AXIS2_PLACEMENT_3D ( 'NONE', #17116, #22051, #21724 ) ;
#17084 = FACE_OUTER_BOUND ( 'NONE', #2884, .T. ) ;
#17085 = AXIS2_PLACEMENT_3D ( 'NONE', #17089, #15407, #82 ) ;
#17086 = CIRCLE ( 'NONE', #8862, 4.193574995607837863 ) ;
#17087 = ADVANCED_FACE ( 'NONE', ( #18045 ), #7072, .T. ) ;
#17088 = ORIENTED_EDGE ( 'NONE', *, *, #1782, .T. ) ;
#17089 = CARTESIAN_POINT ( 'NONE',  ( 1.724728116533979616, 43.26054587065083012, 31.80876104995653719 ) ) ;
#17090 = ADVANCED_FACE ( 'NONE', ( #18281 ), #21437, .T. ) ;
#17091 = LINE ( 'NONE', #5465, #16731 ) ;
#17092 = EDGE_CURVE ( 'NONE', #1545, #1750, #15982, .T. ) ;
#17093 = CARTESIAN_POINT ( 'NONE',  ( 9.641460742840918030, -32.61873716947361856, 68.00000000000000000 ) ) ;
#17094 = VECTOR ( 'NONE', #15793, 1000.000000000000000 ) ;
#17095 = CARTESIAN_POINT ( 'NONE',  ( 29.13662752439705272, 0.000000000000000000, 1.500000000000001332 ) ) ;
#17096 = ORIENTED_EDGE ( 'NONE', *, *, #3600, .F. ) ;
#17097 = CARTESIAN_POINT ( 'NONE',  ( 23.02398829872514341, 2.245853328535763360, 13.29652846991536563 ) ) ;
#17098 = AXIS2_PLACEMENT_3D ( 'NONE', #10589, #20347, #15609 ) ;
#17099 = CARTESIAN_POINT ( 'NONE',  ( -18.22752199202934520, -39.04634676501046187, 13.50000000000000000 ) ) ;
#17100 = CARTESIAN_POINT ( 'NONE',  ( 30.79999999999999716, -84.70000000000001705, 0.3000000000000033751 ) ) ;
#17101 = ORIENTED_EDGE ( 'NONE', *, *, #623, .T. ) ;
#17102 = DIRECTION ( 'NONE',  ( -0.000000000000000000, -0.000000000000000000, -1.000000000000000000 ) ) ;
#17103 = DIRECTION ( 'NONE',  ( 3.491481338843133355E-15, -1.000000000000000000, -4.275831445896958607E-31 ) ) ;
#17104 = TOROIDAL_SURFACE ( 'NONE', #20981, 0.5000000000000000000, 0.2500000000000000000 ) ;
#17105 = VECTOR ( 'NONE', #15122, 1000.000000000000000 ) ;
#17106 = VERTEX_POINT ( 'NONE', #16583 ) ;
#17107 = CARTESIAN_POINT ( 'NONE',  ( -34.40000000000001279, 85.00000000000000000, 80.00000000000000000 ) ) ;
#17108 = CARTESIAN_POINT ( 'NONE',  ( -4.127054932750482408, 32.93424481021354921, 7.321391277662001151 ) ) ;
#17109 = EDGE_LOOP ( 'NONE', ( #5477, #14889 ) ) ;
#17110 = VECTOR ( 'NONE', #1769, 1000.000000000000000 ) ;
#17111 = ORIENTED_EDGE ( 'NONE', *, *, #20301, .F. ) ;
#17112 = DIRECTION ( 'NONE',  ( -1.000000000000000000, 0.000000000000000000, 0.000000000000000000 ) ) ;
#17113 = CIRCLE ( 'NONE', #8541, 0.05000000000000143219 ) ;
#17114 = ORIENTED_EDGE ( 'NONE', *, *, #6252, .T. ) ;
#17115 = EDGE_CURVE ( 'NONE', #7135, #8671, #9894, .T. ) ;
#17116 = CARTESIAN_POINT ( 'NONE',  ( -3.127054932750481964, -32.93424481021354921, 68.00000000000000000 ) ) ;
#17117 = ORIENTED_EDGE ( 'NONE', *, *, #3317, .F. ) ;
#17118 = CARTESIAN_POINT ( 'NONE',  ( 25.37540678000429040, -36.74634676501047181, 13.50000000000000000 ) ) ;
#17119 = EDGE_CURVE ( 'NONE', #8171, #10037, #1050, .T. ) ;
#17120 = AXIS2_PLACEMENT_3D ( 'NONE', #14380, #12587, #9036 ) ;
#17121 = FACE_OUTER_BOUND ( 'NONE', #16681, .T. ) ;
#17122 = DIRECTION ( 'NONE',  ( 0.000000000000000000, 0.000000000000000000, 1.000000000000000000 ) ) ;
#17123 = DIRECTION ( 'NONE',  ( 0.000000000000000000, -1.000000000000000000, 0.000000000000000000 ) ) ;
#17124 = DIRECTION ( 'NONE',  ( 1.000000000000000000, -0.000000000000000000, 0.000000000000000000 ) ) ;
#17125 = DIRECTION ( 'NONE',  ( -0.000000000000000000, 1.000000000000000000, 0.000000000000000000 ) ) ;
#17126 = DIRECTION ( 'NONE',  ( 0.000000000000000000, 0.000000000000000000, 1.000000000000000000 ) ) ;
#17127 = ORIENTED_EDGE ( 'NONE', *, *, #3559, .T. ) ;
#17128 = CARTESIAN_POINT ( 'NONE',  ( 1.724728116533979616, 43.26054587065083012, 47.80876104995653719 ) ) ;
#17129 = DIRECTION ( 'NONE',  ( 0.000000000000000000, 0.000000000000000000, -1.000000000000000000 ) ) ;
#17130 = DIRECTION ( 'NONE',  ( 0.000000000000000000, 0.000000000000000000, 1.000000000000000000 ) ) ;
#17131 = ADVANCED_FACE ( 'NONE', ( #11339 ), #22103, .T. ) ;
#17132 = DIRECTION ( 'NONE',  ( 0.000000000000000000, 1.000000000000000000, 0.000000000000000000 ) ) ;
#17133 = ORIENTED_EDGE ( 'NONE', *, *, #8723, .F. ) ;
#17134 = ORIENTED_EDGE ( 'NONE', *, *, #20885, .F. ) ;
#17135 = ORIENTED_EDGE ( 'NONE', *, *, #1363, .T. ) ;
#17136 = VECTOR ( 'NONE', #22058, 1000.000000000000000 ) ;
#17137 = EDGE_CURVE ( 'NONE', #16854, #1535, #9923, .T. ) ;
#17138 = ORIENTED_EDGE ( 'NONE', *, *, #15428, .F. ) ;
#17139 = VERTEX_POINT ( 'NONE', #11995 ) ;
#17140 = CARTESIAN_POINT ( 'NONE',  ( -31.26086011588027347, 83.95073979834609190, 68.50000000000000000 ) ) ;
#17141 = FACE_OUTER_BOUND ( 'NONE', #4741, .T. ) ;
#17142 = CARTESIAN_POINT ( 'NONE',  ( -23.32398829872514057, 2.157133568460765538, 13.50000000000000000 ) ) ;
#17143 = CARTESIAN_POINT ( 'NONE',  ( -34.40000000000001279, 85.00000000000000000, 79.39999999999999147 ) ) ;
#17144 = AXIS2_PLACEMENT_3D ( 'NONE', #20413, #19157, #7202 ) ;
#17145 = LINE ( 'NONE', #16919, #6198 ) ;
#17146 = CIRCLE ( 'NONE', #14632, 1.162443609680678280 ) ;
#17147 = CYLINDRICAL_SURFACE ( 'NONE', #15065, 0.05000000000000143219 ) ;
#17148 = DIRECTION ( 'NONE',  ( 0.000000000000000000, -1.000000000000000000, 0.000000000000000000 ) ) ;
#17149 = CARTESIAN_POINT ( 'NONE',  ( 1.774728116533979660, 43.31054587065082728, 53.66679706732590915 ) ) ;
#17150 = EDGE_CURVE ( 'NONE', #9296, #12289, #1328, .T. ) ;
#17151 = DIRECTION ( 'NONE',  ( 1.000000000000000000, 0.000000000000000000, 0.000000000000000000 ) ) ;
#17152 = ORIENTED_EDGE ( 'NONE', *, *, #733, .T. ) ;
#17153 = ORIENTED_EDGE ( 'NONE', *, *, #4070, .F. ) ;
#17154 = DIRECTION ( 'NONE',  ( 0.000000000000000000, 1.000000000000000000, -0.000000000000000000 ) ) ;
#17155 = DIRECTION ( 'NONE',  ( -6.123233995736764803E-17, -0.000000000000000000, 1.000000000000000000 ) ) ;
#17156 = VERTEX_POINT ( 'NONE', #16816 ) ;
#17157 = ADVANCED_FACE ( 'NONE', ( #15247 ), #9208, .T. ) ;
#17158 = AXIS2_PLACEMENT_3D ( 'NONE', #3189, #3069, #1601 ) ;
#17159 = EDGE_CURVE ( 'NONE', #14847, #4254, #18838, .T. ) ;
#17160 = CIRCLE ( 'NONE', #18585, 0.05000000000000143219 ) ;
#17161 = EDGE_CURVE ( 'NONE', #15492, #13894, #15033, .T. ) ;
#17162 = PRODUCT_DEFINITION_SHAPE ( 'NONE', 'NONE',  #5212 ) ;
#17163 = DIRECTION ( 'NONE',  ( -0.000000000000000000, 1.000000000000000000, -0.000000000000000000 ) ) ;
#17164 = ADVANCED_FACE ( 'NONE', ( #11661 ), #16927, .F. ) ;
#17165 = DIRECTION ( 'NONE',  ( 0.000000000000000000, 0.000000000000000000, 1.000000000000000000 ) ) ;
#17166 = DIRECTION ( 'NONE',  ( 1.000000000000000000, 0.000000000000000000, 0.000000000000000000 ) ) ;
#17167 = ORIENTED_EDGE ( 'NONE', *, *, #15760, .F. ) ;
#17168 = DIRECTION ( 'NONE',  ( 1.000000000000000000, 0.000000000000000000, 0.000000000000000000 ) ) ;
#17169 = DIRECTION ( 'NONE',  ( 0.000000000000000000, -1.000000000000000000, 0.000000000000000000 ) ) ;
#17170 = DIRECTION ( 'NONE',  ( 0.000000000000000000, -1.000000000000000000, 0.000000000000000000 ) ) ;
#17171 = DIRECTION ( 'NONE',  ( 0.000000000000000000, 0.000000000000000000, 1.000000000000000000 ) ) ;
#17172 = CARTESIAN_POINT ( 'NONE',  ( -9.141460742840918030, -33.43424481021354921, 68.00000000000000000 ) ) ;
#17173 = AXIS2_PLACEMENT_3D ( 'NONE', #21284, #12866, #14099 ) ;
#17174 = EDGE_CURVE ( 'NONE', #4799, #488, #21015, .T. ) ;
#17175 = VERTEX_POINT ( 'NONE', #13458 ) ;
#17176 = CARTESIAN_POINT ( 'NONE',  ( 9.141460742840918030, -33.43424481021354921, 42.50000000000000000 ) ) ;
#17177 = PRESENTATION_LAYER_ASSIGNMENT (  '', '', ( #18599 ) ) ;
#17178 = DIRECTION ( 'NONE',  ( 1.000000000000000000, 0.000000000000000000, 0.000000000000000000 ) ) ;
#17179 = CARTESIAN_POINT ( 'NONE',  ( 1.724728116533979616, 43.26054587065083012, 35.80876104995653009 ) ) ;
#17180 = ORIENTED_EDGE ( 'NONE', *, *, #9536, .T. ) ;
#17181 = VERTEX_POINT ( 'NONE', #20635 ) ;
#17182 = VERTEX_POINT ( 'NONE', #10226 ) ;
#17183 = DIRECTION ( 'NONE',  ( -1.000000000000000000, -0.000000000000000000, -0.000000000000000000 ) ) ;
#17184 = CARTESIAN_POINT ( 'NONE',  ( 0.000000000000000000, 85.00000000000000000, 79.70000000000000284 ) ) ;
#17185 = DIRECTION ( 'NONE',  ( 0.000000000000000000, -1.000000000000000000, 0.000000000000000000 ) ) ;
#17186 = EDGE_CURVE ( 'NONE', #21823, #12212, #20298, .T. ) ;
#17187 = VERTEX_POINT ( 'NONE', #15472 ) ;
#17188 = CARTESIAN_POINT ( 'NONE',  ( -9.718906393579157310, 44.91645089659918710, 70.88527860057354246 ) ) ;
#17189 = EDGE_CURVE ( 'NONE', #6840, #14859, #6659, .T. ) ;
#17190 = ORIENTED_EDGE ( 'NONE', *, *, #16619, .F. ) ;
#17191 = CARTESIAN_POINT ( 'NONE',  ( -1.824728116533986810, 43.31054587065082728, 47.80876104995653719 ) ) ;
#17192 = CIRCLE ( 'NONE', #20067, 1.299999999999999156 ) ;
#17193 = DIRECTION ( 'NONE',  ( -1.000000000000000000, 0.000000000000000000, -0.000000000000000000 ) ) ;
#17194 = CARTESIAN_POINT ( 'NONE',  ( 4.127054932750481520, 33.43424481021354921, 42.50000000000000000 ) ) ;
#17195 = DIRECTION ( 'NONE',  ( -1.000000000000000000, -0.000000000000000000, -0.000000000000000000 ) ) ;
#17196 = VERTEX_POINT ( 'NONE', #8668 ) ;
#17197 = CYLINDRICAL_SURFACE ( 'NONE', #5595, 5.000000000000004441 ) ;
#17198 = DIRECTION ( 'NONE',  ( 0.000000000000000000, 0.000000000000000000, -1.000000000000000000 ) ) ;
#17199 = CIRCLE ( 'NONE', #6152, 1.000000000000000888 ) ;
#17200 = DIRECTION ( 'NONE',  ( 0.000000000000000000, 0.000000000000000000, 1.000000000000000000 ) ) ;
#17201 = CARTESIAN_POINT ( 'NONE',  ( 33.19999999999999574, -84.70000000000001705, 1.799999999999996048 ) ) ;
#17202 = EDGE_LOOP ( 'NONE', ( #1849, #21107, #12925, #5461 ) ) ;
#17203 =( NAMED_UNIT ( * ) PLANE_ANGLE_UNIT ( ) SI_UNIT ( $, .RADIAN. ) );
#17204 = AXIS2_PLACEMENT_3D ( 'NONE', #5411, #1476, #11765 ) ;
#17205 = CIRCLE ( 'NONE', #12187, 0.2500000000000002220 ) ;
#17206 = CIRCLE ( 'NONE', #18990, 5.000000000000004441 ) ;
#17207 = CARTESIAN_POINT ( 'NONE',  ( 31.44597781366222122, 0.000000000000000000, 68.50000000000000000 ) ) ;
#17208 = VERTEX_POINT ( 'NONE', #139 ) ;
#17209 = CARTESIAN_POINT ( 'NONE',  ( 31.69597781366222122, 58.94165929845684104, 70.50000000000000000 ) ) ;
#17210 = ADVANCED_FACE ( 'NONE', ( #6559 ), #19946, .T. ) ;
#17211 = CYLINDRICAL_SURFACE ( 'NONE', #7444, 1.000000000000000888 ) ;
#17212 = VERTEX_POINT ( 'NONE', #17041 ) ;
#17213 = ORIENTED_EDGE ( 'NONE', *, *, #17605, .F. ) ;
#17214 = VERTEX_POINT ( 'NONE', #12111 ) ;
#17215 = AXIS2_PLACEMENT_3D ( 'NONE', #14046, #290, #5466 ) ;
#17216 = EDGE_CURVE ( 'NONE', #9183, #6237, #3269, .T. ) ;
#17217 = CIRCLE ( 'NONE', #18286, 0.2500000000000002220 ) ;
#17218 = ORIENTED_EDGE ( 'NONE', *, *, #21774, .T. ) ;
#17219 = CARTESIAN_POINT ( 'NONE',  ( 29.05186365738250842, 0.05288320938007240457, 0.000000000000000000 ) ) ;
#17220 = TOROIDAL_SURFACE ( 'NONE', #21885, 0.05000000000000000278, 0.05000000000000000278 ) ;
#17221 = VECTOR ( 'NONE', #18162, 1000.000000000000000 ) ;
#17222 = FACE_OUTER_BOUND ( 'NONE', #19632, .T. ) ;
#17223 = CARTESIAN_POINT ( 'NONE',  ( -17.45292532278785913, 0.000000000000000000, 68.00000000000000000 ) ) ;
#17224 = DIRECTION ( 'NONE',  ( 0.000000000000000000, 1.000000000000000000, -0.000000000000000000 ) ) ;
#17225 = CARTESIAN_POINT ( 'NONE',  ( -1.724728116533986721, 43.26054587065083012, 43.80876104995653719 ) ) ;
#17226 = CYLINDRICAL_SURFACE ( 'NONE', #17944, 0.5000000000000004441 ) ;
#17227 = ORIENTED_EDGE ( 'NONE', *, *, #20766, .F. ) ;
#17228 = VECTOR ( 'NONE', #18978, 1000.000000000000000 ) ;
#17229 = ADVANCED_FACE ( 'NONE', ( #8224 ), #3183, .T. ) ;
#17230 = DIRECTION ( 'NONE',  ( -1.000000000000000000, -0.000000000000000000, -0.000000000000000000 ) ) ;
#17231 = FACE_OUTER_BOUND ( 'NONE', #2177, .T. ) ;
#17232 = CIRCLE ( 'NONE', #8305, 0.3000000000000016542 ) ;
#17233 = LINE ( 'NONE', #14, #186 ) ;
#17234 = EDGE_CURVE ( 'NONE', #21381, #8248, #628, .T. ) ;
#17235 = ORIENTED_EDGE ( 'NONE', *, *, #12667, .T. ) ;
#17236 = ORIENTED_EDGE ( 'NONE', *, *, #2405, .T. ) ;
#17237 = CYLINDRICAL_SURFACE ( 'NONE', #8886, 0.5000000000000004441 ) ;
#17238 = PRODUCT_CONTEXT ( 'NONE', #1985, 'mechanical' ) ;
#17239 = ORIENTED_EDGE ( 'NONE', *, *, #10827, .F. ) ;
#17240 = AXIS2_PLACEMENT_3D ( 'NONE', #2479, #21516, #891 ) ;
#17241 = DIRECTION ( 'NONE',  ( 0.000000000000000000, 1.000000000000000000, -0.000000000000000000 ) ) ;
#17242 = ORIENTED_EDGE ( 'NONE', *, *, #15976, .F. ) ;
#17243 = ORIENTED_EDGE ( 'NONE', *, *, #2727, .T. ) ;
#17244 = DIRECTION ( 'NONE',  ( 0.000000000000000000, 0.000000000000000000, -1.000000000000000000 ) ) ;
#17245 = LINE ( 'NONE', #12196, #9879 ) ;
#17246 = EDGE_CURVE ( 'NONE', #17318, #21351, #3131, .T. ) ;
#17247 = CARTESIAN_POINT ( 'NONE',  ( 1.724728116533979616, 43.26054587065083012, 49.76679706732591058 ) ) ;
#17248 = CARTESIAN_POINT ( 'NONE',  ( 0.000000000000000000, 43.31054587065082728, 4.000000000000000000 ) ) ;
#17249 = CARTESIAN_POINT ( 'NONE',  ( -23.02398829872525710, 2.334689865870841263, 13.36916081092377873 ) ) ;
#17250 = CARTESIAN_POINT ( 'NONE',  ( 30.07540678000427548, -63.74634676501045050, 7.200000000000000178 ) ) ;
#17251 = CARTESIAN_POINT ( 'NONE',  ( -29.37540678000427619, 5.000000000000000000, 3.799999999999999822 ) ) ;
#17252 = CARTESIAN_POINT ( 'NONE',  ( 17.45292532278785913, 38.74634676501045760, 13.79999999999999893 ) ) ;
#17253 = EDGE_CURVE ( 'NONE', #8060, #814, #8765, .T. ) ;
#17254 = EDGE_CURVE ( 'NONE', #2496, #8891, #2035, .T. ) ;
#17255 = DIRECTION ( 'NONE',  ( 4.336808689941893885E-15, 0.000000000000000000, 1.000000000000000000 ) ) ;
#17256 = VERTEX_POINT ( 'NONE', #9089 ) ;
#17257 = VERTEX_POINT ( 'NONE', #8881 ) ;
#17258 = DIRECTION ( 'NONE',  ( 0.000000000000000000, 1.000000000000000000, -0.000000000000000000 ) ) ;
#17259 = LINE ( 'NONE', #20959, #2757 ) ;
#17260 = EDGE_LOOP ( 'NONE', ( #18444, #4736, #16961, #22098 ) ) ;
#17261 = CARTESIAN_POINT ( 'NONE',  ( -10.73004499984425664, -2.546852060775805615, 68.50000000000000000 ) ) ;
#17262 = ADVANCED_FACE ( 'NONE', ( #17687 ), #4938, .F. ) ;
#17263 = CARTESIAN_POINT ( 'NONE',  ( 33.50000000000000000, 85.00000000000000000, 1.200000000000004174 ) ) ;
#17264 = STYLED_ITEM ( 'NONE', ( #899 ), #13111 ) ;
#17265 = CARTESIAN_POINT ( 'NONE',  ( 31.50000000000002132, -71.70000000000001705, 3.500000000000000000 ) ) ;
#17266 = EDGE_LOOP ( 'NONE', ( #17641, #4064, #13706, #9605 ) ) ;
#17267 = DIRECTION ( 'NONE',  ( -0.000000000000000000, -0.000000000000000000, 1.000000000000000000 ) ) ;
#17268 = LINE ( 'NONE', #1843, #18538 ) ;
#17269 = DIRECTION ( 'NONE',  ( 0.000000000000000000, 0.000000000000000000, 1.000000000000000000 ) ) ;
#17270 = PLANE ( 'NONE',  #8026 ) ;
#17271 = PRESENTATION_STYLE_ASSIGNMENT (( #15486 ) ) ;
#17272 = DIRECTION ( 'NONE',  ( 0.000000000000000000, 0.000000000000000000, -1.000000000000000000 ) ) ;
#17273 = CARTESIAN_POINT ( 'NONE',  ( 29.37540678000427619, -6.000000000000000000, 7.500000000000000000 ) ) ;
#17274 = EDGE_CURVE ( 'NONE', #11635, #19777, #4165, .T. ) ;
#17275 = EDGE_CURVE ( 'NONE', #2212, #9069, #15567, .T. ) ;
#17276 = ORIENTED_EDGE ( 'NONE', *, *, #1267, .T. ) ;
#17277 = CARTESIAN_POINT ( 'NONE',  ( -14.71174975910705029, 51.61873716947361856, 14.00000000000000000 ) ) ;
#17278 = DIRECTION ( 'NONE',  ( 0.000000000000000000, 1.000000000000000000, 0.000000000000000000 ) ) ;
#17279 = EDGE_CURVE ( 'NONE', #14452, #14817, #21382, .T. ) ;
#17280 = CARTESIAN_POINT ( 'NONE',  ( 1.724728116533979616, 42.36054587065083155, 31.80876104995653719 ) ) ;
#17281 = ORIENTED_EDGE ( 'NONE', *, *, #19214, .T. ) ;
#17282 = ORIENTED_EDGE ( 'NONE', *, *, #22146, .F. ) ;
#17283 = ORIENTED_EDGE ( 'NONE', *, *, #21196, .F. ) ;
#17284 = FACE_OUTER_BOUND ( 'NONE', #20609, .T. ) ;
#17285 = DIRECTION ( 'NONE',  ( -3.052134192567367925E-16, -1.000000000000000000, 0.000000000000000000 ) ) ;
#17286 =( REPRESENTATION_RELATIONSHIP ('NONE','NONE', #561, #9407 ) REPRESENTATION_RELATIONSHIP_WITH_TRANSFORMATION ( #21168 )SHAPE_REPRESENTATION_RELATIONSHIP( ) );
#17287 = VECTOR ( 'NONE', #15000, 1000.000000000000000 ) ;
#17288 = DIRECTION ( 'NONE',  ( 0.000000000000000000, 1.000000000000000000, 0.000000000000000000 ) ) ;
#17289 = VERTEX_POINT ( 'NONE', #7104 ) ;
#17290 = CARTESIAN_POINT ( 'NONE',  ( -1.724728116533986721, 42.31054587065082728, 49.71679706732589921 ) ) ;
#17291 = EDGE_CURVE ( 'NONE', #4773, #19066, #14940, .T. ) ;
#17292 = ORIENTED_EDGE ( 'NONE', *, *, #9504, .T. ) ;
#17293 = DIRECTION ( 'NONE',  ( 1.000000000000000000, -0.000000000000000000, 0.000000000000000000 ) ) ;
#17294 = LINE ( 'NONE', #11816, #6396 ) ;
#17295 = DIRECTION ( 'NONE',  ( 0.000000000000000000, 0.000000000000000000, 1.000000000000000000 ) ) ;
#17296 = DIRECTION ( 'NONE',  ( 0.000000000000000000, 0.000000000000000000, 1.000000000000000000 ) ) ;
#17297 = ORIENTED_EDGE ( 'NONE', *, *, #8254, .T. ) ;
#17298 = DIRECTION ( 'NONE',  ( -1.000000000000000000, 0.000000000000000000, 0.000000000000000000 ) ) ;
#17299 = DIRECTION ( 'NONE',  ( 1.000000000000000000, 0.000000000000000000, 0.000000000000000000 ) ) ;
#17300 = CARTESIAN_POINT ( 'NONE',  ( -17.92752199202934094, -50.11873716947361856, 13.79999999999999893 ) ) ;
#17301 = DIRECTION ( 'NONE',  ( 1.000000000000000000, -0.000000000000000000, 0.000000000000000000 ) ) ;
#17302 = ORIENTED_EDGE ( 'NONE', *, *, #7882, .T. ) ;
#17303 = DIRECTION ( 'NONE',  ( 1.000000000000000000, 0.000000000000000000, -1.224646799147353207E-16 ) ) ;
#17304 = EDGE_CURVE ( 'NONE', #13966, #16058, #15686, .T. ) ;
#17305 = EDGE_LOOP ( 'NONE', ( #6636, #4586, #21434, #18278 ) ) ;
#17306 = EDGE_CURVE ( 'NONE', #11011, #497, #4587, .T. ) ;
#17307 = DIRECTION ( 'NONE',  ( -1.000000000000000000, 0.000000000000000000, -0.000000000000000000 ) ) ;
#17308 = ORIENTED_EDGE ( 'NONE', *, *, #6241, .F. ) ;
#17309 = ORIENTED_EDGE ( 'NONE', *, *, #12884, .T. ) ;
#17311 = EDGE_CURVE ( 'NONE', #6000, #11560, #2066, .T. ) ;
#17310 = CARTESIAN_POINT ( 'NONE',  ( -1.724728116533986721, 42.36054587065083155, 41.71679706732590631 ) ) ;
#17312 = CARTESIAN_POINT ( 'NONE',  ( -6.728906393579160650, 43.00645089659919762, 70.88527860057354246 ) ) ;
#17313 = VERTEX_POINT ( 'NONE', #2368 ) ;
#17314 = EDGE_LOOP ( 'NONE', ( #5675, #3055, #160, #12627 ) ) ;
#17315 = CIRCLE ( 'NONE', #20911, 0.2999999999999999334 ) ;
#17316 = AXIS2_PLACEMENT_3D ( 'NONE', #2360, #9524, #562 ) ;
#17317 = EDGE_CURVE ( 'NONE', #11274, #21172, #14564, .T. ) ;
#17318 = VERTEX_POINT ( 'NONE', #17594 ) ;
#17319 = DIRECTION ( 'NONE',  ( -3.052134192567367925E-16, 1.000000000000000000, -0.000000000000000000 ) ) ;
#17320 = DIRECTION ( 'NONE',  ( 1.000000000000000000, 0.000000000000000000, 0.000000000000000000 ) ) ;
#17321 = DIRECTION ( 'NONE',  ( 0.000000000000000000, -1.000000000000000000, 0.000000000000000000 ) ) ;
#17322 = EDGE_CURVE ( 'NONE', #3983, #21319, #10548, .T. ) ;
#17323 = ORIENTED_EDGE ( 'NONE', *, *, #11850, .F. ) ;
#17324 = CARTESIAN_POINT ( 'NONE',  ( 29.42075962687198754, 2.605814368445832141, 0.09348339755409348917 ) ) ;
#17325 = LINE ( 'NONE', #16191, #14251 ) ;
#17326 = DIRECTION ( 'NONE',  ( 0.000000000000000000, 0.000000000000000000, 1.000000000000000000 ) ) ;
#17327 = CIRCLE ( 'NONE', #534, 0.2500000000000002220 ) ;
#17328 = CIRCLE ( 'NONE', #16244, 0.05000000000000143219 ) ;
#17329 = EDGE_CURVE ( 'NONE', #9447, #16467, #569, .T. ) ;
#17330 = VERTEX_POINT ( 'NONE', #17365 ) ;
#17331 = CARTESIAN_POINT ( 'NONE',  ( -1.724728116533986721, 42.36054587065083155, 47.80876104995653719 ) ) ;
#17332 = CARTESIAN_POINT ( 'NONE',  ( -14.66174975910705136, 51.76873716947361714, 13.50000000000000000 ) ) ;
#17333 = EDGE_LOOP ( 'NONE', ( #1562, #20820, #17239, #21060 ) ) ;
#17334 = ORIENTED_EDGE ( 'NONE', *, *, #6994, .T. ) ;
#17335 = DIRECTION ( 'NONE',  ( -1.000000000000000000, 0.000000000000000000, 0.000000000000000000 ) ) ;
#17336 = DIRECTION ( 'NONE',  ( 0.000000000000000000, 0.000000000000000000, 1.000000000000000000 ) ) ;
#17337 = ORIENTED_EDGE ( 'NONE', *, *, #11702, .F. ) ;
#17338 = ORIENTED_EDGE ( 'NONE', *, *, #18680, .T. ) ;
#17339 = DIRECTION ( 'NONE',  ( 0.000000000000000000, 0.000000000000000000, -1.000000000000000000 ) ) ;
#17340 = EDGE_LOOP ( 'NONE', ( #19388, #17535, #1517, #8533 ) ) ;
#17341 = CIRCLE ( 'NONE', #2351, 1.826718556943725202 ) ;
#17342 = AXIS2_PLACEMENT_3D ( 'NONE', #11689, #13483, #11796 ) ;
#17343 = VECTOR ( 'NONE', #7031, 1000.000000000000000 ) ;
#17344 = ORIENTED_EDGE ( 'NONE', *, *, #126, .F. ) ;
#17345 = DIRECTION ( 'NONE',  ( -0.000000000000000000, -1.000000000000000000, -0.000000000000000000 ) ) ;
#17346 = ADVANCED_FACE ( 'NONE', ( #14339 ), #359, .T. ) ;
#17347 = CARTESIAN_POINT ( 'NONE',  ( -25.37540678000426908, 38.74634676501045760, 13.79999999999999893 ) ) ;
#17348 = CARTESIAN_POINT ( 'NONE',  ( 0.000000000000000000, -51.61873716947361856, 14.00000000000000000 ) ) ;
#17349 = EDGE_CURVE ( 'NONE', #13615, #6266, #10666, .T. ) ;
#17350 = LINE ( 'NONE', #4355, #11023 ) ;
#17351 = CARTESIAN_POINT ( 'NONE',  ( 30.67540678000428045, -63.74634676501045050, 3.500000000000000000 ) ) ;
#17352 = CARTESIAN_POINT ( 'NONE',  ( -1.824728116533986810, 43.31054587065082728, 53.76679706732590347 ) ) ;
#17353 = CARTESIAN_POINT ( 'NONE',  ( -1.724728116533986721, 42.36054587065083155, 31.80876104995653719 ) ) ;
#17354 = LINE ( 'NONE', #5522, #19119 ) ;
#17355 = DIRECTION ( 'NONE',  ( 1.000000000000000000, 0.000000000000000000, 0.000000000000000000 ) ) ;
#17356 = AXIS2_PLACEMENT_3D ( 'NONE', #679, #10862, #20620 ) ;
#17357 = AXIS2_PLACEMENT_3D ( 'NONE', #4312, #17837, #4198 ) ;
#17358 = VECTOR ( 'NONE', #7964, 1000.000000000000000 ) ;
#17359 = DIRECTION ( 'NONE',  ( 0.000000000000000000, -0.000000000000000000, -1.000000000000000000 ) ) ;
#17360 = LINE ( 'NONE', #2032, #11124 ) ;
#17361 = AXIS2_PLACEMENT_3D ( 'NONE', #7774, #4300, #17939 ) ;
#17362 = EDGE_LOOP ( 'NONE', ( #18551, #3528, #20251, #9537 ) ) ;
#17363 = VECTOR ( 'NONE', #8234, 1000.000000000000000 ) ;
#17364 = VERTEX_POINT ( 'NONE', #2152 ) ;
#17365 = CARTESIAN_POINT ( 'NONE',  ( -17.45292532278785913, -34.11873716947361856, 68.50000000000000000 ) ) ;
#17366 = CARTESIAN_POINT ( 'NONE',  ( 29.05186365738250842, 0.05288320938007240457, 0.2999999999999947153 ) ) ;
#17367 = VERTEX_POINT ( 'NONE', #9200 ) ;
#17368 = ORIENTED_EDGE ( 'NONE', *, *, #18402, .F. ) ;
#17369 = CIRCLE ( 'NONE', #2731, 0.5000000000000004441 ) ;
#17370 = VECTOR ( 'NONE', #10036, 1000.000000000000000 ) ;
#17371 = TOROIDAL_SURFACE ( 'NONE', #3462, 3.200000000000003286, 0.2999999999999999889 ) ;
#17372 = EDGE_CURVE ( 'NONE', #9450, #10373, #461, .T. ) ;
#17373 = DIRECTION ( 'NONE',  ( -2.388292521039847891E-16, 0.000000000000000000, -1.000000000000000000 ) ) ;
#17374 = FACE_OUTER_BOUND ( 'NONE', #21440, .T. ) ;
#17375 = TOROIDAL_SURFACE ( 'NONE', #15578, 0.05000000000000000278, 0.05000000000000000278 ) ;
#17376 = EDGE_LOOP ( 'NONE', ( #19142, #14461, #8240, #5510 ) ) ;
#17377 = FACE_OUTER_BOUND ( 'NONE', #15340, .T. ) ;
#17378 = CARTESIAN_POINT ( 'NONE',  ( -1.824728116533986810, 42.36054587065083155, 27.80876104995653719 ) ) ;
#17379 = CARTESIAN_POINT ( 'NONE',  ( -23.32398829872514057, 5.683640910026983128, 13.50000000000000000 ) ) ;
#17380 = CARTESIAN_POINT ( 'NONE',  ( 29.20000000000002061, 2.848961824869257864, 0.000000000000000000 ) ) ;
#17381 = DIRECTION ( 'NONE',  ( 1.000000000000000000, 0.000000000000000000, 0.000000000000000000 ) ) ;
#17382 = DIRECTION ( 'NONE',  ( 0.000000000000000000, 0.000000000000000000, -1.000000000000000000 ) ) ;
#17383 = CARTESIAN_POINT ( 'NONE',  ( 15.21174975910707161, -41.81054587065082728, 68.50000000000000000 ) ) ;
#17384 = VERTEX_POINT ( 'NONE', #4060 ) ;
#17385 = DIRECTION ( 'NONE',  ( 0.000000000000000000, -1.000000000000000000, 0.000000000000000000 ) ) ;
#17386 = CYLINDRICAL_SURFACE ( 'NONE', #13757, 2.500000000000002220 ) ;
#17387 = VECTOR ( 'NONE', #8336, 1000.000000000000000 ) ;
#17388 = EDGE_LOOP ( 'NONE', ( #11536, #14411, #3652, #3392, #14681 ) ) ;
#17389 = AXIS2_PLACEMENT_3D ( 'NONE', #9745, #12962, #14866 ) ;
#17390 = AXIS2_PLACEMENT_3D ( 'NONE', #15916, #594, #14254 ) ;
#17391 = EDGE_LOOP ( 'NONE', ( #13240, #1783, #13320, #18618 ) ) ;
#17392 = VERTEX_POINT ( 'NONE', #10877 ) ;
#17393 = CARTESIAN_POINT ( 'NONE',  ( -17.95292532278785913, -50.11873716947361856, 13.99999999999999822 ) ) ;
#17394 = FACE_OUTER_BOUND ( 'NONE', #12929, .T. ) ;
#17395 = LINE ( 'NONE', #15600, #20376 ) ;
#17396 = AXIS2_PLACEMENT_3D ( 'NONE', #91, #3113, #6494 ) ;
#17397 = CARTESIAN_POINT ( 'NONE',  ( -22.16013893094044462, 45.60883947780118319, 68.25000000000000000 ) ) ;
#17398 = AXIS2_PLACEMENT_3D ( 'NONE', #1856, #20448, #18531 ) ;
#17399 = ORIENTED_EDGE ( 'NONE', *, *, #5957, .F. ) ;
#17400 = DIRECTION ( 'NONE',  ( 0.000000000000000000, 0.000000000000000000, 1.000000000000000000 ) ) ;
#17401 = EDGE_CURVE ( 'NONE', #13878, #9395, #642, .T. ) ;
#17402 = ORIENTED_EDGE ( 'NONE', *, *, #9622, .T. ) ;
#17403 = LINE ( 'NONE', #14044, #2437 ) ;
#17404 = CIRCLE ( 'NONE', #4187, 2.500000000000002220 ) ;
#17405 = EDGE_CURVE ( 'NONE', #21160, #21055, #20062, .T. ) ;
#17406 = DIRECTION ( 'NONE',  ( 1.000000000000000000, 0.000000000000000000, 0.000000000000000000 ) ) ;
#17407 = VECTOR ( 'NONE', #17293, 1000.000000000000000 ) ;
#17408 = VECTOR ( 'NONE', #14639, 1000.000000000000000 ) ;
#17409 = CYLINDRICAL_SURFACE ( 'NONE', #3229, 0.2500000000000002220 ) ;
#17410 = DIRECTION ( 'NONE',  ( 1.000000000000000000, -0.000000000000000000, 0.000000000000000000 ) ) ;
#17411 = ORIENTED_EDGE ( 'NONE', *, *, #6612, .T. ) ;
#17412 = LINE ( 'NONE', #14049, #5975 ) ;
#17413 = VECTOR ( 'NONE', #824, 1000.000000000000000 ) ;
#17414 = DIRECTION ( 'NONE',  ( -0.000000000000000000, -1.000000000000000000, -0.000000000000000000 ) ) ;
#17415 = DIRECTION ( 'NONE',  ( 0.000000000000000000, 1.000000000000000000, 0.000000000000000000 ) ) ;
#17416 = EDGE_LOOP ( 'NONE', ( #20155, #7495, #15406, #8025 ) ) ;
#17417 = AXIS2_PLACEMENT_3D ( 'NONE', #4409, #2852, #16246 ) ;
#17418 = AXIS2_PLACEMENT_3D ( 'NONE', #1349, #18138, #12976 ) ;
#17419 = VERTEX_POINT ( 'NONE', #21746 ) ;
#17420 = CARTESIAN_POINT ( 'NONE',  ( 15.21174975910707161, -32.10873716947361345, 68.25000000000000000 ) ) ;
#17421 = CYLINDRICAL_SURFACE ( 'NONE', #4502, 0.3000000000000016542 ) ;
#17422 = ORIENTED_EDGE ( 'NONE', *, *, #17329, .F. ) ;
#17423 = ORIENTED_EDGE ( 'NONE', *, *, #10702, .T. ) ;
#17424 = CARTESIAN_POINT ( 'NONE',  ( -1.724728116533986721, 43.26054587065083012, 33.66679706732590915 ) ) ;
#17425 = EDGE_CURVE ( 'NONE', #6365, #13377, #7874, .T. ) ;
#17426 = CARTESIAN_POINT ( 'NONE',  ( -24.94594744299175915, 42.46645089659918426, 68.25000000000000000 ) ) ;
#17427 = AXIS2_PLACEMENT_3D ( 'NONE', #6731, #9962, #1443 ) ;
#17428 = VECTOR ( 'NONE', #14596, 1000.000000000000000 ) ;
#17429 = VECTOR ( 'NONE', #4019, 1000.000000000000000 ) ;
#17430 = ORIENTED_EDGE ( 'NONE', *, *, #16497, .T. ) ;
#17431 = CIRCLE ( 'NONE', #4585, 3.800000000000004707 ) ;
#17432 = VERTEX_POINT ( 'NONE', #16562 ) ;
#17433 = AXIS2_PLACEMENT_3D ( 'NONE', #4282, #14555, #7753 ) ;
#17434 = AXIS2_PLACEMENT_3D ( 'NONE', #1900, #5285, #16903 ) ;
#17435 = EDGE_CURVE ( 'NONE', #9735, #15755, #1720, .T. ) ;
#17436 = EDGE_CURVE ( 'NONE', #2755, #9735, #10985, .T. ) ;
#17437 = ORIENTED_EDGE ( 'NONE', *, *, #5406, .T. ) ;
#17438 = FACE_OUTER_BOUND ( 'NONE', #21270, .T. ) ;
#17439 = EDGE_CURVE ( 'NONE', #16241, #20933, #17798, .T. ) ;
#17440 = CARTESIAN_POINT ( 'NONE',  ( -10.20831163238817219, 41.92645089659918511, 70.88527860057354246 ) ) ;
#17441 = ADVANCED_FACE ( 'NONE', ( #21413 ), #12756, .T. ) ;
#17442 = DIRECTION ( 'NONE',  ( 1.000000000000000000, -0.000000000000000000, 0.000000000000000000 ) ) ;
#17443 = UNCERTAINTY_MEASURE_WITH_UNIT (LENGTH_MEASURE( 1.000000000000000082E-05 ), #5320, 'distance_accuracy_value', 'NONE');
#17444 = VERTEX_POINT ( 'NONE', #4388 ) ;
#17445 = CIRCLE ( 'NONE', #17085, 0.1000000000000028644 ) ;
#17446 = VECTOR ( 'NONE', #20028, 1000.000000000000000 ) ;
#17447 = CYLINDRICAL_SURFACE ( 'NONE', #13202, 0.2999999999999999334 ) ;
#17448 = AXIS2_PLACEMENT_3D ( 'NONE', #15582, #5100, #10026 ) ;
#17449 = DIRECTION ( 'NONE',  ( 0.000000000000000000, -1.000000000000000000, 0.000000000000000000 ) ) ;
#17450 = AXIS2_PLACEMENT_3D ( 'NONE', #3898, #7253, #7358 ) ;
#17451 = DIRECTION ( 'NONE',  ( 0.9510565162951554186, -1.164708318489094811E-16, 0.3090169943749414561 ) ) ;
#17452 = VECTOR ( 'NONE', #12844, 1000.000000000000000 ) ;
#17453 = AXIS2_PLACEMENT_3D ( 'NONE', #5525, #20847, #7307 ) ;
#17454 = VERTEX_POINT ( 'NONE', #9314 ) ;
#17455 = ADVANCED_FACE ( 'NONE', ( #14436 ), #2598, .T. ) ;
#17456 = CARTESIAN_POINT ( 'NONE',  ( 32.20000000000001705, 71.00000000000001421, 3.500000000000000000 ) ) ;
#17457 = CARTESIAN_POINT ( 'NONE',  ( 1.724728116533979616, 43.31054587065082728, 31.80876104995653719 ) ) ;
#17458 = EDGE_LOOP ( 'NONE', ( #15450, #12772, #20780, #16807 ) ) ;
#17459 = EDGE_LOOP ( 'NONE', ( #9987, #8491, #15147 ) ) ;
#17460 = ORIENTED_EDGE ( 'NONE', *, *, #18469, .T. ) ;
#17461 = DIRECTION ( 'NONE',  ( 0.000000000000000000, -0.000000000000000000, 1.000000000000000000 ) ) ;
#17462 = EDGE_LOOP ( 'NONE', ( #14948, #17101, #16745, #4218 ) ) ;
#17463 = AXIS2_PLACEMENT_3D ( 'NONE', #4101, #2090, #3900 ) ;
#17464 = DIRECTION ( 'NONE',  ( 1.000000000000000000, -0.000000000000000000, 0.000000000000000000 ) ) ;
#17465 = ORIENTED_EDGE ( 'NONE', *, *, #10260, .T. ) ;
#17466 = VECTOR ( 'NONE', #11135, 1000.000000000000000 ) ;
#17467 = EDGE_CURVE ( 'NONE', #21328, #20804, #2936, .T. ) ;
#17468 = ORIENTED_EDGE ( 'NONE', *, *, #11208, .F. ) ;
#17469 = VECTOR ( 'NONE', #9471, 1000.000000000000000 ) ;
#17470 = ADVANCED_FACE ( 'NONE', ( #21633 ), #14781, .T. ) ;
#17471 = CARTESIAN_POINT ( 'NONE',  ( -17.95292532278785913, 38.74634676501045760, 42.50000000000000000 ) ) ;
#17472 = CARTESIAN_POINT ( 'NONE',  ( 29.20000000000002061, 0.000000000000000000, 0.2999999999999947153 ) ) ;
#17473 = CARTESIAN_POINT ( 'NONE',  ( 33.19999999999999574, -85.00000000000000000, 78.20000000000000284 ) ) ;
#17474 = DIRECTION ( 'NONE',  ( -1.000000000000000000, 0.000000000000000000, -0.000000000000000000 ) ) ;
#17475 = CARTESIAN_POINT ( 'NONE',  ( 28.71290943744531177, 6.649236572130504896, 13.47739020623642325 ) ) ;
#17476 = CARTESIAN_POINT ( 'NONE',  ( 1.774728116533979438, 42.31054587065082728, 31.80876104995653719 ) ) ;
#17477 = DIRECTION ( 'NONE',  ( -1.000000000000000000, 0.000000000000000000, 0.000000000000000000 ) ) ;
#17478 = DIRECTION ( 'NONE',  ( 0.000000000000000000, 1.000000000000000000, 0.000000000000000000 ) ) ;
#17479 = DIRECTION ( 'NONE',  ( -0.4461977533474359436, -1.523483689126226091E-15, -0.8949343913984425525 ) ) ;
#17480 = VERTEX_POINT ( 'NONE', #2696 ) ;
#17481 = ORIENTED_EDGE ( 'NONE', *, *, #20069, .F. ) ;
#17482 = CARTESIAN_POINT ( 'NONE',  ( 1.774728116533973665, 42.31054587065082728, 4.000000000000000000 ) ) ;
#17483 = SURFACE_STYLE_USAGE ( .BOTH. , #8669 ) ;
#17485 = ADVANCED_FACE ( 'NONE', ( #9534 ), #9941, .T. ) ;
#17484 = DIRECTION ( 'NONE',  ( -1.000000000000000000, 0.000000000000000000, 0.000000000000000000 ) ) ;
#17486 = EDGE_CURVE ( 'NONE', #15569, #15927, #8177, .T. ) ;
#17487 = ORIENTED_EDGE ( 'NONE', *, *, #19380, .T. ) ;
#17488 = VERTEX_POINT ( 'NONE', #16221 ) ;
#17489 = AXIS2_PLACEMENT_3D ( 'NONE', #12010, #9006, #15907 ) ;
#17490 = ADVANCED_FACE ( 'NONE', ( #18141 ), #9763, .T. ) ;
#17491 = VECTOR ( 'NONE', #9613, 1000.000000000000000 ) ;
#17492 = DIRECTION ( 'NONE',  ( -1.000000000000000000, 0.000000000000000000, 1.224646799147353207E-16 ) ) ;
#17493 = AXIS2_PLACEMENT_3D ( 'NONE', #9767, #1237, #16226 ) ;
#17494 = CIRCLE ( 'NONE', #19292, 0.3000000000000016542 ) ;
#17495 = DIRECTION ( 'NONE',  ( -0.000000000000000000, -0.000000000000000000, -1.000000000000000000 ) ) ;
#17496 = EDGE_LOOP ( 'NONE', ( #16261, #14797, #10809, #6775, #17411 ) ) ;
#17497 = CARTESIAN_POINT ( 'NONE',  ( 9.141460742840918030, 33.93424481021354921, 68.50000000000000000 ) ) ;
#17498 = CARTESIAN_POINT ( 'NONE',  ( 15.21174975910705918, 51.86873716947361856, 13.05380965755522737 ) ) ;
#17499 = DIRECTION ( 'NONE',  ( 0.000000000000000000, 0.000000000000000000, 1.000000000000000000 ) ) ;
#17500 = DIRECTION ( 'NONE',  ( -0.000000000000000000, 0.000000000000000000, -1.000000000000000000 ) ) ;
#17501 = DIRECTION ( 'NONE',  ( 0.000000000000000000, 0.000000000000000000, -1.000000000000000000 ) ) ;
#17502 = LINE ( 'NONE', #156, #13061 ) ;
#17503 = CARTESIAN_POINT ( 'NONE',  ( 1.774728116533979438, 42.31054587065082728, 39.80876104995653719 ) ) ;
#17504 = ORIENTED_EDGE ( 'NONE', *, *, #16178, .T. ) ;
#17505 = DIRECTION ( 'NONE',  ( -0.000000000000000000, -0.000000000000000000, -1.000000000000000000 ) ) ;
#17506 = CARTESIAN_POINT ( 'NONE',  ( 15.21174975910705918, -52.39333383871510108, 13.79999999999999893 ) ) ;
#17507 = CARTESIAN_POINT ( 'NONE',  ( -15.95292532278785913, -52.11873716947361856, 68.50000000000000000 ) ) ;
#17508 = ORIENTED_EDGE ( 'NONE', *, *, #18821, .T. ) ;
#17509 = ORIENTED_EDGE ( 'NONE', *, *, #11208, .T. ) ;
#17510 = ORIENTED_EDGE ( 'NONE', *, *, #7203, .F. ) ;
#17511 = CARTESIAN_POINT ( 'NONE',  ( 18.22752199202934520, 50.11873716947361856, 13.79999999999999893 ) ) ;
#17512 = AXIS2_PLACEMENT_3D ( 'NONE', #16592, #1263, #18051 ) ;
#17514 = EDGE_CURVE ( 'NONE', #7220, #1252, #16345, .T. ) ;
#17513 = DIRECTION ( 'NONE',  ( 0.000000000000000000, 0.000000000000000000, 1.000000000000000000 ) ) ;
#17515 = AXIS2_PLACEMENT_3D ( 'NONE', #18765, #15410, #13176 ) ;
#17516 = ORIENTED_EDGE ( 'NONE', *, *, #15926, .T. ) ;
#17517 = CIRCLE ( 'NONE', #9669, 1.500000000000001332 ) ;
#17518 = EDGE_CURVE ( 'NONE', #20718, #16569, #8085, .T. ) ;
#17519 = DIRECTION ( 'NONE',  ( 1.224646799147353207E-16, 0.000000000000000000, 1.000000000000000000 ) ) ;
#17520 = VERTEX_POINT ( 'NONE', #13096 ) ;
#17521 = LINE ( 'NONE', #4090, #8943 ) ;
#17522 = FACE_OUTER_BOUND ( 'NONE', #9044, .T. ) ;
#17523 = ORIENTED_EDGE ( 'NONE', *, *, #10730, .T. ) ;
#17524 = FACE_OUTER_BOUND ( 'NONE', #20340, .T. ) ;
#17525 = DIRECTION ( 'NONE',  ( 1.000000000000000000, 0.000000000000000000, 0.000000000000000000 ) ) ;
#17526 = DIRECTION ( 'NONE',  ( 0.000000000000000000, 1.000000000000000000, 0.000000000000000000 ) ) ;
#17527 = SPHERICAL_SURFACE ( 'NONE', #15205, 0.2500000000000000000 ) ;
#17528 = ORIENTED_EDGE ( 'NONE', *, *, #22111, .F. ) ;
#17529 = DIRECTION ( 'NONE',  ( -1.000000000000000000, 0.000000000000000000, 0.000000000000000000 ) ) ;
#17530 = DIRECTION ( 'NONE',  ( 0.000000000000000000, -1.000000000000000000, 0.000000000000000000 ) ) ;
#17531 = CIRCLE ( 'NONE', #7901, 0.04999999999999991257 ) ;
#17532 = CIRCLE ( 'NONE', #1441, 0.1000000000000028644 ) ;
#17533 = DIRECTION ( 'NONE',  ( 1.000000000000000000, 0.000000000000000000, 0.000000000000000000 ) ) ;
#17534 = CARTESIAN_POINT ( 'NONE',  ( -15.95292532278785913, 51.61873716947361856, 14.00000000000000000 ) ) ;
#17535 = ORIENTED_EDGE ( 'NONE', *, *, #10874, .F. ) ;
#17536 = EDGE_CURVE ( 'NONE', #14127, #2103, #19953, .T. ) ;
#17537 = CARTESIAN_POINT ( 'NONE',  ( 29.50000000000002132, -69.00000000000000000, 1.500000000000000000 ) ) ;
#17538 = EDGE_LOOP ( 'NONE', ( #4135, #15269, #8407, #16362 ) ) ;
#17539 = CYLINDRICAL_SURFACE ( 'NONE', #4817, 0.2500000000000002220 ) ;
#17540 = CARTESIAN_POINT ( 'NONE',  ( -30.79999999999999361, -85.00000000000000000, 1.499999999999999556 ) ) ;
#17541 = ORIENTED_EDGE ( 'NONE', *, *, #10782, .T. ) ;
#17542 = EDGE_LOOP ( 'NONE', ( #16568, #13348, #14728, #7453 ) ) ;
#17543 = FACE_OUTER_BOUND ( 'NONE', #6215, .T. ) ;
#17544 = EDGE_CURVE ( 'NONE', #1750, #17812, #19236, .T. ) ;
#17545 = EDGE_CURVE ( 'NONE', #15319, #19806, #15998, .T. ) ;
#17546 = DIRECTION ( 'NONE',  ( 1.000000000000000000, 0.000000000000000000, 0.000000000000000000 ) ) ;
#17547 = ORIENTED_EDGE ( 'NONE', *, *, #4594, .T. ) ;
#17548 = CIRCLE ( 'NONE', #13256, 0.2999999999999947153 ) ;
#17549 = VERTEX_POINT ( 'NONE', #13553 ) ;
#17550 = ORIENTED_EDGE ( 'NONE', *, *, #10627, .T. ) ;
#17551 = DIRECTION ( 'NONE',  ( -0.000000000000000000, -0.000000000000000000, -1.000000000000000000 ) ) ;
#17552 = CARTESIAN_POINT ( 'NONE',  ( 15.21174975910707161, 41.81054587065082728, 68.25000000000000000 ) ) ;
#17553 = CARTESIAN_POINT ( 'NONE',  ( 28.87540678000427619, 6.494748934539263274, 7.799999999999999822 ) ) ;
#17554 = DIRECTION ( 'NONE',  ( 0.000000000000000000, -1.000000000000000000, 0.000000000000000000 ) ) ;
#17555 = ADVANCED_FACE ( 'NONE', ( #5169 ), #9229, .T. ) ;
#17556 = CIRCLE ( 'NONE', #15092, 0.2999999999999999334 ) ;
#17557 = AXIS2_PLACEMENT_3D ( 'NONE', #17277, #19080, #1942 ) ;
#17558 = CARTESIAN_POINT ( 'NONE',  ( 15.21174975910707161, -51.61873716947361856, 68.50000000000000000 ) ) ;
#17559 = VERTEX_POINT ( 'NONE', #9983 ) ;
#17560 = DIRECTION ( 'NONE',  ( 1.000000000000000000, 0.000000000000000000, 0.000000000000000000 ) ) ;
#17561 = DIRECTION ( 'NONE',  ( -0.000000000000000000, -1.000000000000000000, -0.000000000000000000 ) ) ;
#17562 = DIRECTION ( 'NONE',  ( -1.000000000000000000, 0.000000000000000000, 0.000000000000000000 ) ) ;
#17563 = EDGE_LOOP ( 'NONE', ( #13269, #13143, #17190, #11051 ) ) ;
#17564 = EDGE_CURVE ( 'NONE', #5485, #9706, #11533, .T. ) ;
#17565 = FACE_OUTER_BOUND ( 'NONE', #16065, .T. ) ;
#17566 = ORIENTED_EDGE ( 'NONE', *, *, #12072, .F. ) ;
#17567 = CIRCLE ( 'NONE', #9340, 0.5000000000000004441 ) ;
#17568 = EDGE_CURVE ( 'NONE', #13360, #19336, #8308, .T. ) ;
#17569 = ORIENTED_EDGE ( 'NONE', *, *, #8035, .F. ) ;
#17570 = CARTESIAN_POINT ( 'NONE',  ( 23.02398829872513986, 2.157133568460765538, 13.19999999999999929 ) ) ;
#17571 = CONTEXT_DEPENDENT_SHAPE_REPRESENTATION ( #7724, #6630 ) ;
#17572 = CIRCLE ( 'NONE', #16848, 6.800000000000000711 ) ;
#17573 = EDGE_LOOP ( 'NONE', ( #19871, #19391, #18139, #10383 ) ) ;
#17574 = ORIENTED_EDGE ( 'NONE', *, *, #7050, .F. ) ;
#17575 = CARTESIAN_POINT ( 'NONE',  ( -23.75488095381848197, 42.46645089659918426, 13.74999999999999822 ) ) ;
#17576 = EDGE_LOOP ( 'NONE', ( #21342, #5168, #10425, #11312 ) ) ;
#17577 = VERTEX_POINT ( 'NONE', #4730 ) ;
#17578 = DIRECTION ( 'NONE',  ( -0.000000000000000000, -1.000000000000000000, 0.000000000000000000 ) ) ;
#17579 = CARTESIAN_POINT ( 'NONE',  ( -33.20000000000001705, 84.70000000000001705, 78.20000000000000284 ) ) ;
#17580 = EDGE_CURVE ( 'NONE', #877, #22102, #8520, .T. ) ;
#17581 = CARTESIAN_POINT ( 'NONE',  ( -30.19999999999999574, 69.70000000000001705, 9.999999999999998224 ) ) ;
#17582 = DIRECTION ( 'NONE',  ( 0.000000000000000000, -0.000000000000000000, -1.000000000000000000 ) ) ;
#17583 = FACE_OUTER_BOUND ( 'NONE', #21056, .T. ) ;
#17584 = APPLICATION_CONTEXT ( 'automotive_design' ) ;
#17585 = AXIS2_PLACEMENT_3D ( 'NONE', #12532, #19479, #20845 ) ;
#17586 = DIRECTION ( 'NONE',  ( 0.000000000000000000, -1.000000000000000000, 0.000000000000000000 ) ) ;
#17587 = CARTESIAN_POINT ( 'NONE',  ( 1.724728116533979838, 42.36054587065083155, 49.71679706732590631 ) ) ;
#17588 = FACE_OUTER_BOUND ( 'NONE', #22015, .T. ) ;
#17589 = DIRECTION ( 'NONE',  ( 0.000000000000000000, 1.000000000000000000, 0.000000000000000000 ) ) ;
#17590 = ADVANCED_FACE ( 'NONE', ( #13325 ), #22073, .T. ) ;
#17591 = ADVANCED_FACE ( 'NONE', ( #8528 ), #10097, .T. ) ;
#17592 = ORIENTED_EDGE ( 'NONE', *, *, #3017, .T. ) ;
#17593 = ORIENTED_EDGE ( 'NONE', *, *, #1216, .T. ) ;
#17594 = CARTESIAN_POINT ( 'NONE',  ( 29.50000000000002132, -2.473451120191013430, 1.500000000000001332 ) ) ;
#17595 = EDGE_CURVE ( 'NONE', #18889, #20015, #22107, .T. ) ;
#17596 = DIRECTION ( 'NONE',  ( -0.000000000000000000, -0.000000000000000000, -1.000000000000000000 ) ) ;
#17597 = ORIENTED_EDGE ( 'NONE', *, *, #17435, .F. ) ;
#17598 = ORIENTED_EDGE ( 'NONE', *, *, #17253, .T. ) ;
#17599 = AXIS2_PLACEMENT_3D ( 'NONE', #10950, #11170, #12839 ) ;
#17600 = FACE_BOUND ( 'NONE', #10262, .T. ) ;
#17601 = CARTESIAN_POINT ( 'NONE',  ( 25.37540678000426908, 36.74634676501047181, 42.50000000000000000 ) ) ;
#17602 = ORIENTED_EDGE ( 'NONE', *, *, #2656, .T. ) ;
#17603 = DIRECTION ( 'NONE',  ( 0.000000000000000000, 0.000000000000000000, 1.000000000000000000 ) ) ;
#17604 = DIRECTION ( 'NONE',  ( 0.000000000000000000, 0.000000000000000000, -1.000000000000000000 ) ) ;
#17605 = EDGE_CURVE ( 'NONE', #8891, #22102, #20161, .T. ) ;
#17606 = CARTESIAN_POINT ( 'NONE',  ( 15.21174975910705918, 52.11873716947361856, 14.00000000000000000 ) ) ;
#17607 = DIRECTION ( 'NONE',  ( -0.000000000000000000, 1.000000000000000000, 0.000000000000000000 ) ) ;
#17608 = CARTESIAN_POINT ( 'NONE',  ( -14.66895125224955621, 51.92349729544097414, 13.49999999999999822 ) ) ;
#17609 = DIRECTION ( 'NONE',  ( 0.000000000000000000, 0.000000000000000000, 1.000000000000000000 ) ) ;
#17610 = DIRECTION ( 'NONE',  ( 0.000000000000000000, 0.000000000000000000, 1.000000000000000000 ) ) ;
#17611 = LINE ( 'NONE', #2280, #1253 ) ;
#17612 = CARTESIAN_POINT ( 'NONE',  ( 29.50000000000002132, -69.00000000000000000, 0.2999999999999947153 ) ) ;
#17613 = ORIENTED_EDGE ( 'NONE', *, *, #17921, .T. ) ;
#17614 = ORIENTED_EDGE ( 'NONE', *, *, #1895, .T. ) ;
#17615 = ORIENTED_EDGE ( 'NONE', *, *, #19340, .F. ) ;
#17616 = CARTESIAN_POINT ( 'NONE',  ( 27.77120804565220169, -2.094189496455408861, 0.2999999999999947153 ) ) ;
#17617 = EDGE_CURVE ( 'NONE', #15052, #823, #3264, .T. ) ;
#17618 = CARTESIAN_POINT ( 'NONE',  ( -9.178906393579158163, 42.46645089659918426, 70.88527860057354246 ) ) ;
#17619 = DIRECTION ( 'NONE',  ( -0.9729678061520345977, -0.2309407893631976461, 0.000000000000000000 ) ) ;
#17620 = ORIENTED_EDGE ( 'NONE', *, *, #9622, .F. ) ;
#17621 = FACE_OUTER_BOUND ( 'NONE', #12870, .T. ) ;
#17622 = DIRECTION ( 'NONE',  ( 1.000000000000000000, -0.000000000000000000, -0.000000000000000000 ) ) ;
#17623 = ORIENTED_EDGE ( 'NONE', *, *, #11585, .F. ) ;
#17624 = CYLINDRICAL_SURFACE ( 'NONE', #9576, 0.5000000000000004441 ) ;
#17625 = DIRECTION ( 'NONE',  ( 0.000000000000000000, 0.000000000000000000, 1.000000000000000000 ) ) ;
#17626 = CARTESIAN_POINT ( 'NONE',  ( 34.39999999999998437, 85.00000000000000000, 80.00000000000000000 ) ) ;
#17627 = CARTESIAN_POINT ( 'NONE',  ( -9.141460742840918030, 33.43424481021354921, 42.50000000000000000 ) ) ;
#17628 = ORIENTED_EDGE ( 'NONE', *, *, #8365, .F. ) ;
#17629 = CARTESIAN_POINT ( 'NONE',  ( -17.95292532278785913, 0.000000000000000000, 109.6002446535588319 ) ) ;
#17630 = CARTESIAN_POINT ( 'NONE',  ( -34.39999999999999858, -84.70000000000001705, 0.6000000000000033085 ) ) ;
#17631 = ADVANCED_FACE ( 'NONE', ( #8643 ), #10201, .F. ) ;
#17632 = DIRECTION ( 'NONE',  ( 0.000000000000000000, 0.000000000000000000, 1.000000000000000000 ) ) ;
#17633 = ORIENTED_EDGE ( 'NONE', *, *, #16295, .F. ) ;
#17634 = ADVANCED_FACE ( 'NONE', ( #3487 ), #5694, .T. ) ;
#17635 =( LENGTH_UNIT ( ) NAMED_UNIT ( * ) SI_UNIT ( .MILLI., .METRE. ) );
#17636 = ORIENTED_EDGE ( 'NONE', *, *, #18421, .T. ) ;
#17637 = CYLINDRICAL_SURFACE ( 'NONE', #10535, 0.5000000000000004441 ) ;
#17638 = LINE ( 'NONE', #7364, #565 ) ;
#17639 =( GEOMETRIC_REPRESENTATION_CONTEXT ( 3 ) GLOBAL_UNCERTAINTY_ASSIGNED_CONTEXT ( ( #13856 ) ) GLOBAL_UNIT_ASSIGNED_CONTEXT ( ( #7209, #12309, #18022 ) ) REPRESENTATION_CONTEXT ( 'NONE', 'WORKASPACE' ) );
#17640 = ORIENTED_EDGE ( 'NONE', *, *, #15099, .T. ) ;
#17641 = ORIENTED_EDGE ( 'NONE', *, *, #13520, .F. ) ;
#17642 = CYLINDRICAL_SURFACE ( 'NONE', #9608, 0.2999999999999999334 ) ;
#17643 = DIRECTION ( 'NONE',  ( -0.000000000000000000, -1.000000000000000000, -0.000000000000000000 ) ) ;
#17644 = VERTEX_POINT ( 'NONE', #1352 ) ;
#17645 = VERTEX_POINT ( 'NONE', #8202 ) ;
#17646 = ADVANCED_FACE ( 'NONE', ( #10321 ), #18520, .T. ) ;
#17647 = EDGE_LOOP ( 'NONE', ( #10292, #4770, #5419, #8495 ) ) ;
#17648 = CARTESIAN_POINT ( 'NONE',  ( -30.67540678000428045, 0.000000000000000000, 3.799999999999999822 ) ) ;
#17649 = AXIS2_PLACEMENT_3D ( 'NONE', #3473, #17125, #8297 ) ;
#17650 = CARTESIAN_POINT ( 'NONE',  ( -15.95292532278785913, 51.61873716947361856, 68.00000000000000000 ) ) ;
#17651 = AXIS2_PLACEMENT_3D ( 'NONE', #18517, #3200, #16834 ) ;
#17652 = DIRECTION ( 'NONE',  ( 1.000000000000000000, 0.000000000000000000, 0.000000000000000000 ) ) ;
#17653 = DIRECTION ( 'NONE',  ( -0.000000000000000000, -1.000000000000000000, -0.000000000000000000 ) ) ;
#17654 = EDGE_CURVE ( 'NONE', #16620, #2243, #13750, .T. ) ;
#17655 = CARTESIAN_POINT ( 'NONE',  ( 0.000000000000000000, 52.11873716947361856, 109.6002446535588319 ) ) ;
#17656 = ORIENTED_EDGE ( 'NONE', *, *, #14758, .F. ) ;
#17657 = DIRECTION ( 'NONE',  ( 0.000000000000000000, 0.000000000000000000, 1.000000000000000000 ) ) ;
#17658 = CARTESIAN_POINT ( 'NONE',  ( 15.95292532278785913, 50.11873716947361856, 68.00000000000000000 ) ) ;
#17659 = DIRECTION ( 'NONE',  ( 0.000000000000000000, 0.000000000000000000, 1.000000000000000000 ) ) ;
#17660 = VERTEX_POINT ( 'NONE', #16795 ) ;
#17661 = FACE_OUTER_BOUND ( 'NONE', #18076, .T. ) ;
#17662 = EDGE_LOOP ( 'NONE', ( #16700, #20420, #11381, #1645 ) ) ;
#17663 = VERTEX_POINT ( 'NONE', #17570 ) ;
#17664 = ORIENTED_EDGE ( 'NONE', *, *, #19128, .F. ) ;
#17665 = CARTESIAN_POINT ( 'NONE',  ( -25.37540678000427263, 63.74634676501045050, 13.19999999999999929 ) ) ;
#17666 = EDGE_CURVE ( 'NONE', #7269, #21686, #20931, .T. ) ;
#17667 = ORIENTED_EDGE ( 'NONE', *, *, #13261, .F. ) ;
#17668 = VERTEX_POINT ( 'NONE', #7516 ) ;
#17669 = CARTESIAN_POINT ( 'NONE',  ( 15.95292532278785913, 52.09333383871509682, 13.79999999999999893 ) ) ;
#17670 = EDGE_LOOP ( 'NONE', ( #17920, #2488, #8679, #11097 ) ) ;
#17671 = CARTESIAN_POINT ( 'NONE',  ( 29.69597781366221767, 56.94165929845684104, 68.75000000000000000 ) ) ;
#17672 = ORIENTED_EDGE ( 'NONE', *, *, #21139, .F. ) ;
#17673 = ADVANCED_FACE ( 'NONE', ( #5289 ), #17237, .T. ) ;
#17674 = DIRECTION ( 'NONE',  ( 0.000000000000000000, 0.000000000000000000, -1.000000000000000000 ) ) ;
#17675 = LINE ( 'NONE', #9186, #13072 ) ;
#17676 = DIRECTION ( 'NONE',  ( 0.000000000000000000, 0.000000000000000000, 1.000000000000000000 ) ) ;
#17677 = EDGE_CURVE ( 'NONE', #7044, #20727, #2010, .T. ) ;
#17678 = VECTOR ( 'NONE', #19773, 1000.000000000000000 ) ;
#17679 = CARTESIAN_POINT ( 'NONE',  ( 29.69597781366221767, 25.99124249474150972, 70.25000000000000000 ) ) ;
#17680 = CARTESIAN_POINT ( 'NONE',  ( -23.02398829872513986, 2.192121262983578234, 13.33089993820317964 ) ) ;
#17681 = DIRECTION ( 'NONE',  ( 0.000000000000000000, 1.000000000000000000, 0.000000000000000000 ) ) ;
#17682 = DIRECTION ( 'NONE',  ( 0.000000000000000000, 1.000000000000000000, 0.000000000000000000 ) ) ;
#17683 = FACE_BOUND ( 'NONE', #17879, .T. ) ;
#17684 = ORIENTED_EDGE ( 'NONE', *, *, #2808, .F. ) ;
#17685 = AXIS2_PLACEMENT_3D ( 'NONE', #18329, #1100, #13054 ) ;
#17686 = ORIENTED_EDGE ( 'NONE', *, *, #14919, .T. ) ;
#17687 = FACE_OUTER_BOUND ( 'NONE', #22076, .T. ) ;
#17688 = ADVANCED_FACE ( 'NONE', ( #3704 ), #18931, .T. ) ;
#17689 = ORIENTED_EDGE ( 'NONE', *, *, #6044, .F. ) ;
#17690 = VERTEX_POINT ( 'NONE', #10850 ) ;
#17691 = CIRCLE ( 'NONE', #15189, 5.000000000000000888 ) ;
#17692 = AXIS2_PLACEMENT_3D ( 'NONE', #20765, #5545, #1848 ) ;
#17693 = VERTEX_POINT ( 'NONE', #8965 ) ;
#17694 = ADVANCED_FACE ( 'NONE', ( #438 ), #13527, .T. ) ;
#17695 = FACE_OUTER_BOUND ( 'NONE', #18084, .T. ) ;
#17696 = ADVANCED_FACE ( 'NONE', ( #4040 ), #3165, .T. ) ;
#17697 = VECTOR ( 'NONE', #3780, 1000.000000000000000 ) ;
#17698 = CARTESIAN_POINT ( 'NONE',  ( -31.31859531322107770, 84.19398174988410233, 13.50000000000000000 ) ) ;
#17699 = AXIS2_PLACEMENT_3D ( 'NONE', #7248, #16390, #5178 ) ;
#17700 = EDGE_LOOP ( 'NONE', ( #13958, #6977, #21819, #13300 ) ) ;
#17701 = CARTESIAN_POINT ( 'NONE',  ( 31.50000000000002132, -71.70000000000001705, 1.800000000000000044 ) ) ;
#17702 = EDGE_CURVE ( 'NONE', #11864, #18602, #10329, .T. ) ;
#17703 = CYLINDRICAL_SURFACE ( 'NONE', #5369, 0.5000000000000004441 ) ;
#17704 = CARTESIAN_POINT ( 'NONE',  ( -23.61959064016851073, 45.26242829375641463, 13.50000000000000000 ) ) ;
#17705 = CARTESIAN_POINT ( 'NONE',  ( 15.21174975910705918, 52.10286008774955491, 13.87500000000000000 ) ) ;
#17706 = CARTESIAN_POINT ( 'NONE',  ( -15.95292532278785913, -32.11873716947361856, 68.00000000000000000 ) ) ;
#17707 = CARTESIAN_POINT ( 'NONE',  ( -23.02398829872515051, 3.003070052962827141, 13.75712488064577599 ) ) ;
#17708 = AXIS2_PLACEMENT_3D ( 'NONE', #2613, #12998, #19509 ) ;
#17709 = VECTOR ( 'NONE', #1146, 1000.000000000000000 ) ;
#17710 = VECTOR ( 'NONE', #2604, 1000.000000000000000 ) ;
#17711 = ORIENTED_EDGE ( 'NONE', *, *, #12089, .T. ) ;
#17712 = CYLINDRICAL_SURFACE ( 'NONE', #19701, 0.1000000000000028644 ) ;
#17713 = DIRECTION ( 'NONE',  ( 1.000000000000000000, -0.000000000000000000, -0.000000000000000000 ) ) ;
#17714 = FACE_OUTER_BOUND ( 'NONE', #12514, .T. ) ;
#17715 = VERTEX_POINT ( 'NONE', #2343 ) ;
#17716 = ORIENTED_EDGE ( 'NONE', *, *, #18639, .T. ) ;
#17717 = ORIENTED_EDGE ( 'NONE', *, *, #8207, .T. ) ;
#17718 = CARTESIAN_POINT ( 'NONE',  ( -28.90801073195815718, -6.496214187273303686, 7.643093741255248652 ) ) ;
#17719 = CARTESIAN_POINT ( 'NONE',  ( -15.95292532278785913, -32.11873716947361856, 68.00000000000000000 ) ) ;
#17720 = EDGE_CURVE ( 'NONE', #15951, #16703, #4605, .T. ) ;
#17721 = ORIENTED_EDGE ( 'NONE', *, *, #907, .T. ) ;
#17722 = AXIS2_PLACEMENT_3D ( 'NONE', #1767, #13938, #20567 ) ;
#17723 = CIRCLE ( 'NONE', #3797, 0.2999999999999947153 ) ;
#17724 = CARTESIAN_POINT ( 'NONE',  ( -9.178906393579158163, 42.46645089659918426, 74.06027860057353962 ) ) ;
#17725 = AXIS2_PLACEMENT_3D ( 'NONE', #17795, #2475, #11082 ) ;
#17726 = EDGE_CURVE ( 'NONE', #6175, #21952, #9065, .T. ) ;
#17727 = ORIENTED_EDGE ( 'NONE', *, *, #14189, .T. ) ;
#17728 = DIRECTION ( 'NONE',  ( -1.000000000000000000, 0.000000000000000000, 0.000000000000000000 ) ) ;
#17729 = VECTOR ( 'NONE', #21742, 1000.000000000000000 ) ;
#17730 = CARTESIAN_POINT ( 'NONE',  ( 18.22752199202934520, -50.11873716947361856, 13.50000000000000000 ) ) ;
#17731 = CARTESIAN_POINT ( 'NONE',  ( 30.67540678000428045, 6.000000000000000000, 3.500000000000000000 ) ) ;
#17732 = DIRECTION ( 'NONE',  ( 1.000000000000000000, 0.000000000000000000, 0.000000000000000000 ) ) ;
#17733 = CARTESIAN_POINT ( 'NONE',  ( 9.141460742840918030, 33.43424481021354921, 42.50000000000000000 ) ) ;
#17734 = FACE_OUTER_BOUND ( 'NONE', #20930, .T. ) ;
#17735 = ORIENTED_EDGE ( 'NONE', *, *, #3341, .F. ) ;
#17736 = DIRECTION ( 'NONE',  ( 0.000000000000000000, 0.000000000000000000, -1.000000000000000000 ) ) ;
#17737 = EDGE_CURVE ( 'NONE', #19665, #5001, #20324, .T. ) ;
#17738 = CARTESIAN_POINT ( 'NONE',  ( -14.96174975910704852, 41.81054587065082728, 13.62426406871192697 ) ) ;
#17739 = CARTESIAN_POINT ( 'NONE',  ( 1.824728116533979261, 43.26054587065083012, 51.80876104995653719 ) ) ;
#17740 = CARTESIAN_POINT ( 'NONE',  ( 24.13662752439704917, 0.000000000000000000, 7.200000000000000178 ) ) ;
#17741 = ORIENTED_EDGE ( 'NONE', *, *, #4758, .T. ) ;
#17742 = AXIS2_PLACEMENT_3D ( 'NONE', #21889, #9452, #21560 ) ;
#17743 = AXIS2_PLACEMENT_3D ( 'NONE', #20430, #18854, #7115 ) ;
#17744 = AXIS2_PLACEMENT_3D ( 'NONE', #4436, #11247, #18071 ) ;
#17745 = CARTESIAN_POINT ( 'NONE',  ( -29.20000000000002061, 0.000000000000000000, 0.2999999999999947153 ) ) ;
#17746 = TOROIDAL_SURFACE ( 'NONE', #21699, 0.05000000000000000278, 0.05000000000000000278 ) ;
#17747 = ORIENTED_EDGE ( 'NONE', *, *, #18806, .F. ) ;
#17748 = CYLINDRICAL_SURFACE ( 'NONE', #8055, 0.1000000000000028644 ) ;
#17749 = CARTESIAN_POINT ( 'NONE',  ( -31.50000000000002132, -71.00000000000001421, 3.500000000000000000 ) ) ;
#17750 = ORIENTED_EDGE ( 'NONE', *, *, #401, .F. ) ;
#17751 = AXIS2_PLACEMENT_3D ( 'NONE', #7180, #5909, #7691 ) ;
#17752 = VERTEX_POINT ( 'NONE', #12405 ) ;
#17753 = DIRECTION ( 'NONE',  ( 1.000000000000000000, -1.334402673828314029E-15, 0.000000000000000000 ) ) ;
#17754 = CARTESIAN_POINT ( 'NONE',  ( 1.724728116533979616, 42.36054587065083155, 35.75876104995654003 ) ) ;
#17755 = VERTEX_POINT ( 'NONE', #20610 ) ;
#17756 = EDGE_CURVE ( 'NONE', #21336, #11610, #9607, .T. ) ;
#17757 = AXIS2_PLACEMENT_3D ( 'NONE', #7762, #16230, #6202 ) ;
#17758 = EDGE_CURVE ( 'NONE', #8119, #5089, #12084, .T. ) ;
#17759 = VERTEX_POINT ( 'NONE', #3603 ) ;
#17760 = VECTOR ( 'NONE', #6724, 1000.000000000000000 ) ;
#17761 = AXIS2_PLACEMENT_3D ( 'NONE', #2393, #12561, #19630 ) ;
#17762 = ORIENTED_EDGE ( 'NONE', *, *, #17137, .F. ) ;
#17763 = DIRECTION ( 'NONE',  ( 0.000000000000000000, 0.000000000000000000, 1.000000000000000000 ) ) ;
#17764 = VECTOR ( 'NONE', #8670, 1000.000000000000000 ) ;
#17765 = DIRECTION ( 'NONE',  ( 1.000000000000000000, -0.000000000000000000, -0.000000000000000000 ) ) ;
#17766 = VECTOR ( 'NONE', #13002, 1000.000000000000000 ) ;
#17767 = LINE ( 'NONE', #2555, #20814 ) ;
#17768 = CARTESIAN_POINT ( 'NONE',  ( 0.000000000000000000, 4.700000000000000178, 3.500000000000000000 ) ) ;
#17769 = CARTESIAN_POINT ( 'NONE',  ( 29.69597781366221767, 26.24124249474150972, 70.50000000000000000 ) ) ;
#17770 = VERTEX_POINT ( 'NONE', #5736 ) ;
#17771 = CARTESIAN_POINT ( 'NONE',  ( 9.141460742840918030, -32.61873716947361856, 42.50000000000000000 ) ) ;
#17772 = FACE_OUTER_BOUND ( 'NONE', #8626, .T. ) ;
#17773 = DIRECTION ( 'NONE',  ( -0.000000000000000000, 1.000000000000000000, -0.000000000000000000 ) ) ;
#17774 = AXIS2_PLACEMENT_3D ( 'NONE', #20143, #14987, #4924 ) ;
#17775 = AXIS2_PLACEMENT_3D ( 'NONE', #2219, #14179, #21147 ) ;
#17776 = CARTESIAN_POINT ( 'NONE',  ( 31.50000000000002132, 71.00000000000001421, 3.500000000000000000 ) ) ;
#17777 = ORIENTED_EDGE ( 'NONE', *, *, #2656, .F. ) ;
#17778 = DIRECTION ( 'NONE',  ( 0.000000000000000000, 0.000000000000000000, 1.000000000000000000 ) ) ;
#17779 = VERTEX_POINT ( 'NONE', #19139 ) ;
#17780 = AXIS2_PLACEMENT_3D ( 'NONE', #17397, #5562, #17619 ) ;
#17781 = ORIENTED_EDGE ( 'NONE', *, *, #3251, .T. ) ;
#17782 = TOROIDAL_SURFACE ( 'NONE', #17417, 0.7000000000000000666, 0.2999999999999999889 ) ;
#17783 = AXIS2_PLACEMENT_3D ( 'NONE', #7018, #1951, #15397 ) ;
#17784 = CONTEXT_DEPENDENT_SHAPE_REPRESENTATION ( #14861, #4650 ) ;
#17785 = EDGE_CURVE ( 'NONE', #4042, #10367, #8539, .T. ) ;
#17786 = ORIENTED_EDGE ( 'NONE', *, *, #5557, .F. ) ;
#17787 = ORIENTED_EDGE ( 'NONE', *, *, #1416, .F. ) ;
#17788 = ADVANCED_FACE ( 'NONE', ( #7074 ), #13872, .T. ) ;
#17789 = DIRECTION ( 'NONE',  ( 0.000000000000000000, 1.000000000000000000, 0.000000000000000000 ) ) ;
#17790 = ORIENTED_EDGE ( 'NONE', *, *, #572, .F. ) ;
#17791 = CARTESIAN_POINT ( 'NONE',  ( -17.95292532278785913, 38.74634676501045760, 109.6002446535588319 ) ) ;
#17792 = AXIS2_PLACEMENT_3D ( 'NONE', #15502, #171, #13819 ) ;
#17793 = AXIS2_PLACEMENT_3D ( 'NONE', #15627, #17643, #10932 ) ;
#17794 = DIRECTION ( 'NONE',  ( 0.000000000000000000, 0.000000000000000000, 1.000000000000000000 ) ) ;
#17795 = CARTESIAN_POINT ( 'NONE',  ( -33.20000000000000284, 84.70000000000001705, 1.800000000000000266 ) ) ;
#17796 = DIRECTION ( 'NONE',  ( -5.192538640813645496E-17, 1.000000000000000000, 6.359025825921378559E-33 ) ) ;
#17797 = CIRCLE ( 'NONE', #2061, 0.2999999999999999334 ) ;
#17798 = CIRCLE ( 'NONE', #17433, 0.2500000000000002220 ) ;
#17799 = CARTESIAN_POINT ( 'NONE',  ( -15.95292532278785913, 32.11873716947361856, 68.00000000000000000 ) ) ;
#17800 = CIRCLE ( 'NONE', #11716, 0.2999999999999999334 ) ;
#17801 = DIRECTION ( 'NONE',  ( -1.000000000000000000, -0.000000000000000000, -0.000000000000000000 ) ) ;
#17802 = DIRECTION ( 'NONE',  ( -1.000000000000000000, 0.000000000000000000, 0.000000000000000000 ) ) ;
#17804 = ADVANCED_FACE ( 'NONE', ( #2125 ), #18112, .T. ) ;
#17803 = DIRECTION ( 'NONE',  ( 0.000000000000000000, 0.000000000000000000, 1.000000000000000000 ) ) ;
#17805 = CARTESIAN_POINT ( 'NONE',  ( 17.95292532278785913, -38.74634676501046471, 42.50000000000000711 ) ) ;
#17806 = AXIS2_PLACEMENT_3D ( 'NONE', #5924, #5827, #12609 ) ;
#17807 = ORIENTED_EDGE ( 'NONE', *, *, #19626, .F. ) ;
#17808 = VERTEX_POINT ( 'NONE', #19580 ) ;
#17809 = DIRECTION ( 'NONE',  ( 1.000000000000000000, 0.000000000000000000, 0.000000000000000000 ) ) ;
#17810 = EDGE_CURVE ( 'NONE', #20423, #7338, #14643, .T. ) ;
#17811 = AXIS2_PLACEMENT_3D ( 'NONE', #16629, #10277, #5021 ) ;
#17812 = VERTEX_POINT ( 'NONE', #4137 ) ;
#17813 = CIRCLE ( 'NONE', #17453, 4.999999999999997335 ) ;
#17814 = CARTESIAN_POINT ( 'NONE',  ( 14.66918479711007706, -51.92478806352735887, 13.50000000000000000 ) ) ;
#17815 = CARTESIAN_POINT ( 'NONE',  ( 25.37540678000427263, 63.74634676501045050, 13.19999999999999929 ) ) ;
#17816 = ORIENTED_EDGE ( 'NONE', *, *, #15221, .F. ) ;
#17817 = DIRECTION ( 'NONE',  ( -1.000000000000000000, 0.000000000000000000, 0.000000000000000000 ) ) ;
#17818 = EDGE_CURVE ( 'NONE', #15889, #9043, #994, .T. ) ;
#17819 = CARTESIAN_POINT ( 'NONE',  ( 30.19999999999999574, 69.70000000000000284, 1.200000000000003064 ) ) ;
#17820 = CARTESIAN_POINT ( 'NONE',  ( -28.64417692495746692, 6.713479613976641502, 13.50000000000000000 ) ) ;
#17821 = DIRECTION ( 'NONE',  ( -1.000000000000000000, 0.000000000000000000, 0.000000000000000000 ) ) ;
#17822 = DIRECTION ( 'NONE',  ( 2.832483164223434527E-16, -1.000000000000000000, 0.000000000000000000 ) ) ;
#17823 = CIRCLE ( 'NONE', #8915, 0.2999999999999999334 ) ;
#17824 = ORIENTED_EDGE ( 'NONE', *, *, #12215, .F. ) ;
#17825 = CARTESIAN_POINT ( 'NONE',  ( 33.79999999999999005, 85.00000000000000000, 78.50000000000000000 ) ) ;
#17826 = CARTESIAN_POINT ( 'NONE',  ( -29.20000000000002061, -68.70000000000001705, 0.000000000000000000 ) ) ;
#17827 = CARTESIAN_POINT ( 'NONE',  ( 25.37540678000427263, 69.04634676501045476, 3.500000000000000000 ) ) ;
#17828 = ORIENTED_EDGE ( 'NONE', *, *, #14427, .F. ) ;
#17829 = ORIENTED_EDGE ( 'NONE', *, *, #12390, .T. ) ;
#17830 = VERTEX_POINT ( 'NONE', #4468 ) ;
#17831 = DIRECTION ( 'NONE',  ( 1.000000000000000000, 0.000000000000000000, 0.000000000000000000 ) ) ;
#17832 = EDGE_CURVE ( 'NONE', #9069, #13657, #4256, .T. ) ;
#17833 = DIRECTION ( 'NONE',  ( 1.000000000000000000, 0.000000000000000000, 0.000000000000000000 ) ) ;
#17834 = ADVANCED_FACE ( 'NONE', ( #16540 ), #2673, .T. ) ;
#17835 = ORIENTED_EDGE ( 'NONE', *, *, #14689, .F. ) ;
#17836 = ADVANCED_FACE ( 'NONE', ( #14413 ), #14315, .T. ) ;
#17837 = DIRECTION ( 'NONE',  ( 0.000000000000000000, 0.000000000000000000, -1.000000000000000000 ) ) ;
#17838 = ADVANCED_FACE ( 'NONE', ( #16313 ), #11407, .T. ) ;
#17839 = AXIS2_PLACEMENT_3D ( 'NONE', #5079, #239, #20629 ) ;
#17840 = AXIS2_PLACEMENT_3D ( 'NONE', #528, #10742, #17560 ) ;
#17841 = VERTEX_POINT ( 'NONE', #18234 ) ;
#17842 = DIRECTION ( 'NONE',  ( -1.000000000000000000, 0.000000000000000000, 0.000000000000000000 ) ) ;
#17843 = LINE ( 'NONE', #11127, #18823 ) ;
#17844 = DIRECTION ( 'NONE',  ( -0.000000000000000000, 1.000000000000000000, -0.000000000000000000 ) ) ;
#17845 = DIRECTION ( 'NONE',  ( 1.000000000000000000, 0.000000000000000000, 0.000000000000000000 ) ) ;
#17846 = CARTESIAN_POINT ( 'NONE',  ( -9.718906393579157310, 41.42245079618239600, 68.06527860057354928 ) ) ;
#17847 = CARTESIAN_POINT ( 'NONE',  ( 0.000000000000000000, 50.19799549595485644, 13.50000000000000000 ) ) ;
#17848 = VERTEX_POINT ( 'NONE', #2572 ) ;
#17849 = DIRECTION ( 'NONE',  ( 0.000000000000000000, 0.000000000000000000, 1.000000000000000000 ) ) ;
#17850 = DIRECTION ( 'NONE',  ( 1.000000000000000000, 0.000000000000000000, 0.000000000000000000 ) ) ;
#17851 = EDGE_CURVE ( 'NONE', #16066, #15986, #2798, .T. ) ;
#17852 = DIRECTION ( 'NONE',  ( 0.000000000000000000, 1.000000000000000000, 0.000000000000000000 ) ) ;
#17853 = CARTESIAN_POINT ( 'NONE',  ( 0.000000000000000000, 68.44634676501046044, 7.500000000000000000 ) ) ;
#17854 = ORIENTED_EDGE ( 'NONE', *, *, #4636, .T. ) ;
#17855 = FACE_OUTER_BOUND ( 'NONE', #4110, .T. ) ;
#17856 = CARTESIAN_POINT ( 'NONE',  ( 29.37540678000427619, -4.700000000000000178, 3.799999999999999822 ) ) ;
#17857 = VECTOR ( 'NONE', #10266, 1000.000000000000000 ) ;
#17858 = ORIENTED_EDGE ( 'NONE', *, *, #21040, .F. ) ;
#17859 = AXIS2_PLACEMENT_3D ( 'NONE', #11928, #20019, #4686 ) ;
#17860 = CARTESIAN_POINT ( 'NONE',  ( 15.95292532278785913, 50.11873716947361856, 68.00000000000000000 ) ) ;
#17861 = LINE ( 'NONE', #6246, #9880 ) ;
#17862 = VERTEX_POINT ( 'NONE', #2911 ) ;
#17863 = ORIENTED_EDGE ( 'NONE', *, *, #19155, .F. ) ;
#17864 = CARTESIAN_POINT ( 'NONE',  ( 0.000000000000000000, 0.000000000000000000, 70.50000000000000000 ) ) ;
#17865 = DIRECTION ( 'NONE',  ( 0.000000000000000000, -1.000000000000000000, 0.000000000000000000 ) ) ;
#17866 = CYLINDRICAL_SURFACE ( 'NONE', #12414, 0.1000000000000028644 ) ;
#17867 = EDGE_CURVE ( 'NONE', #8633, #7269, #7474, .T. ) ;
#17868 = ORIENTED_EDGE ( 'NONE', *, *, #5817, .T. ) ;
#17869 = EDGE_CURVE ( 'NONE', #18991, #17549, #7108, .T. ) ;
#17870 = ORIENTED_EDGE ( 'NONE', *, *, #16473, .F. ) ;
#17871 = CIRCLE ( 'NONE', #17158, 0.2999999999999999334 ) ;
#17872 = ORIENTED_EDGE ( 'NONE', *, *, #8146, .F. ) ;
#17873 = DIRECTION ( 'NONE',  ( 0.000000000000000000, -0.000000000000000000, -1.000000000000000000 ) ) ;
#17874 = AXIS2_PLACEMENT_3D ( 'NONE', #10976, #14095, #5633 ) ;
#17875 = LINE ( 'NONE', #14398, #15008 ) ;
#17876 = FACE_OUTER_BOUND ( 'NONE', #7388, .T. ) ;
#17877 = DIRECTION ( 'NONE',  ( 1.000000000000000000, 0.000000000000000000, 0.000000000000000000 ) ) ;
#17878 = DIRECTION ( 'NONE',  ( 1.000000000000000000, -0.000000000000000000, -0.000000000000000000 ) ) ;
#17879 = EDGE_LOOP ( 'NONE', ( #5838, #5040, #11574, #11093, #3413, #18250, #1143, #1049 ) ) ;
#17880 = CARTESIAN_POINT ( 'NONE',  ( 31.69597781366222122, 56.94165929845684104, 70.25000000000000000 ) ) ;
#17881 = EDGE_CURVE ( 'NONE', #21087, #4692, #6039, .T. ) ;
#17882 = DIRECTION ( 'NONE',  ( 0.000000000000000000, 1.000000000000000000, 0.000000000000000000 ) ) ;
#17883 = CARTESIAN_POINT ( 'NONE',  ( 14.96174975910707161, 42.31054587065082728, 68.25000000000000000 ) ) ;
#17884 = CARTESIAN_POINT ( 'NONE',  ( 25.37540678000427263, 68.74634676501045760, 7.500000000000000000 ) ) ;
#17885 = AXIS2_PLACEMENT_3D ( 'NONE', #7862, #21515, #1119 ) ;
#17886 = ORIENTED_EDGE ( 'NONE', *, *, #19403, .T. ) ;
#17887 = ORIENTED_EDGE ( 'NONE', *, *, #15105, .T. ) ;
#17888 = ORIENTED_EDGE ( 'NONE', *, *, #4099, .T. ) ;
#17889 = CARTESIAN_POINT ( 'NONE',  ( 29.50000000000002132, 69.00000000000000000, -150.0833101980363722 ) ) ;
#17890 = EDGE_CURVE ( 'NONE', #19133, #18309, #7622, .T. ) ;
#17891 = ORIENTED_EDGE ( 'NONE', *, *, #9474, .F. ) ;
#17892 = ORIENTED_EDGE ( 'NONE', *, *, #18692, .F. ) ;
#17893 = AXIS2_PLACEMENT_3D ( 'NONE', #10793, #9218, #812 ) ;
#17894 = FACE_OUTER_BOUND ( 'NONE', #17391, .T. ) ;
#17895 = ORIENTED_EDGE ( 'NONE', *, *, #2157, .T. ) ;
#17896 = CARTESIAN_POINT ( 'NONE',  ( 25.37540678000427263, 68.44634676501046044, 7.200000000000000178 ) ) ;
#17897 = VECTOR ( 'NONE', #8691, 1000.000000000000000 ) ;
#17898 = ORIENTED_EDGE ( 'NONE', *, *, #22110, .T. ) ;
#17899 = CARTESIAN_POINT ( 'NONE',  ( 25.37540678000427263, -63.74634676501045050, 7.500000000000000000 ) ) ;
#17900 = CARTESIAN_POINT ( 'NONE',  ( -29.50000000000002132, 69.00000000000000000, 0.2999999999999947153 ) ) ;
#17901 = DIRECTION ( 'NONE',  ( 1.000000000000000000, 0.000000000000000000, 0.000000000000000000 ) ) ;
#17902 = VECTOR ( 'NONE', #2965, 1000.000000000000000 ) ;
#17903 = CARTESIAN_POINT ( 'NONE',  ( -14.96174975910705207, 41.81054587065082728, 13.75000000000000000 ) ) ;
#17904 = EDGE_CURVE ( 'NONE', #3783, #9842, #1110, .T. ) ;
#17905 = CARTESIAN_POINT ( 'NONE',  ( 0.000000000000000000, 43.26054587065083012, 47.75876104995653293 ) ) ;
#17906 = VECTOR ( 'NONE', #4071, 1000.000000000000000 ) ;
#17907 = DIRECTION ( 'NONE',  ( -0.000000000000000000, -0.000000000000000000, 1.000000000000000000 ) ) ;
#17908 = EDGE_CURVE ( 'NONE', #20038, #21627, #10961, .T. ) ;
#17909 = CARTESIAN_POINT ( 'NONE',  ( -4.127054932750482408, -33.43424481021354921, 68.50000000000000000 ) ) ;
#17910 = CARTESIAN_POINT ( 'NONE',  ( -8.641460742840918030, 33.43424481021354921, 13.50000000000000000 ) ) ;
#17911 = DIRECTION ( 'NONE',  ( 1.000000000000000000, 0.000000000000000000, 0.000000000000000000 ) ) ;
#17912 = VECTOR ( 'NONE', #16698, 1000.000000000000000 ) ;
#17913 = DIRECTION ( 'NONE',  ( 0.000000000000000000, 0.000000000000000000, 1.000000000000000000 ) ) ;
#17914 = ORIENTED_EDGE ( 'NONE', *, *, #16304, .T. ) ;
#17915 = ORIENTED_EDGE ( 'NONE', *, *, #17720, .T. ) ;
#17916 = DIRECTION ( 'NONE',  ( 0.000000000000000000, 0.000000000000000000, 1.000000000000000000 ) ) ;
#17917 = SURFACE_STYLE_FILL_AREA ( #11096 ) ;
#17918 = CARTESIAN_POINT ( 'NONE',  ( 0.000000000000000000, -52.11873716947361856, 109.6002446535588319 ) ) ;
#17919 = EDGE_LOOP ( 'NONE', ( #8829, #8210, #12848, #14172 ) ) ;
#17920 = ORIENTED_EDGE ( 'NONE', *, *, #19688, .F. ) ;
#17921 = EDGE_CURVE ( 'NONE', #421, #21336, #12743, .T. ) ;
#17922 = TOROIDAL_SURFACE ( 'NONE', #18284, 2.767785046117003489, 0.2500000000000000000 ) ;
#17923 = VECTOR ( 'NONE', #8979, 1000.000000000000000 ) ;
#17924 = CYLINDRICAL_SURFACE ( 'NONE', #8531, 0.2999999999999999334 ) ;
#17925 = CIRCLE ( 'NONE', #14347, 0.05000000000000143219 ) ;
#17926 = CIRCLE ( 'NONE', #1498, 0.5000000000000000000 ) ;
#17927 = AXIS2_PLACEMENT_3D ( 'NONE', #14763, #21505, #6177 ) ;
#17928 = DIRECTION ( 'NONE',  ( 0.000000000000000000, -1.000000000000000000, 0.000000000000000000 ) ) ;
#17929 = ORIENTED_EDGE ( 'NONE', *, *, #17291, .F. ) ;
#17930 = SURFACE_STYLE_USAGE ( .BOTH. , #11444 ) ;
#17931 = ADVANCED_FACE ( 'NONE', ( #21610 ), #21360, .T. ) ;
#17932 = EDGE_CURVE ( 'NONE', #9735, #16845, #16095, .T. ) ;
#17933 = CARTESIAN_POINT ( 'NONE',  ( -29.13662752439705272, 0.000000000000000000, 3.500000000000000000 ) ) ;
#17934 = DIRECTION ( 'NONE',  ( 4.336808689941893885E-15, 0.000000000000000000, 1.000000000000000000 ) ) ;
#17935 = DIRECTION ( 'NONE',  ( -1.000000000000000000, 0.000000000000000000, 0.000000000000000000 ) ) ;
#17936 = CARTESIAN_POINT ( 'NONE',  ( -31.44597781366221412, 27.99124249474150972, 70.50000000000000000 ) ) ;
#17937 = VERTEX_POINT ( 'NONE', #18563 ) ;
#17938 = DIRECTION ( 'NONE',  ( 0.000000000000000000, -0.000000000000000000, -1.000000000000000000 ) ) ;
#17939 = DIRECTION ( 'NONE',  ( 1.000000000000000000, 0.000000000000000000, 0.000000000000000000 ) ) ;
#17940 = ORIENTED_EDGE ( 'NONE', *, *, #8118, .T. ) ;
#17941 = ORIENTED_EDGE ( 'NONE', *, *, #14757, .T. ) ;
#17942 = VERTEX_POINT ( 'NONE', #8178 ) ;
#17943 = CARTESIAN_POINT ( 'NONE',  ( 15.05356361075494576, 52.05881965543597545, 13.87239990309209503 ) ) ;
#17944 = AXIS2_PLACEMENT_3D ( 'NONE', #326, #5730, #1896 ) ;
#17945 = CARTESIAN_POINT ( 'NONE',  ( 15.21174975910705918, 52.39333383871510108, 13.79999999999999893 ) ) ;
#17946 = ORIENTED_EDGE ( 'NONE', *, *, #7273, .T. ) ;
#17947 = VECTOR ( 'NONE', #18398, 1000.000000000000114 ) ;
#17948 = CARTESIAN_POINT ( 'NONE',  ( 31.44597781366222122, 27.99124249474150972, 68.75000000000000000 ) ) ;
#17949 = EDGE_CURVE ( 'NONE', #9183, #7977, #13636, .T. ) ;
#17950 = ORIENTED_EDGE ( 'NONE', *, *, #10730, .F. ) ;
#17951 = PLANE ( 'NONE',  #2548 ) ;
#17952 = PLANE ( 'NONE',  #2785 ) ;
#17953 = CIRCLE ( 'NONE', #4389, 0.1000000000000028644 ) ;
#17954 = CARTESIAN_POINT ( 'NONE',  ( 23.02398829872513630, -2.624937972534827413, 13.63083126556636593 ) ) ;
#17955 = DIRECTION ( 'NONE',  ( 0.000000000000000000, 0.000000000000000000, 1.000000000000000000 ) ) ;
#17956 = CARTESIAN_POINT ( 'NONE',  ( 9.641460742840918030, 32.61873716947361856, 68.50000000000000000 ) ) ;
#17957 = FACE_OUTER_BOUND ( 'NONE', #15093, .T. ) ;
#17958 = EDGE_LOOP ( 'NONE', ( #81, #2216, #18201, #7423 ) ) ;
#17959 = DIRECTION ( 'NONE',  ( 1.000000000000000000, 0.000000000000000000, 0.000000000000000000 ) ) ;
#17960 = DIRECTION ( 'NONE',  ( -2.388292521039847891E-16, -0.000000000000000000, -1.000000000000000000 ) ) ;
#17961 = ADVANCED_FACE ( 'NONE', ( #20244 ), #10173, .T. ) ;
#17962 = EDGE_CURVE ( 'NONE', #21143, #20337, #8502, .T. ) ;
#17963 = EDGE_CURVE ( 'NONE', #21390, #18170, #16769, .T. ) ;
#17964 = DIRECTION ( 'NONE',  ( 1.000000000000000000, 0.000000000000000000, 0.000000000000000000 ) ) ;
#17965 = CARTESIAN_POINT ( 'NONE',  ( -31.69597781366221412, 25.99124249474150972, 70.50000000000000000 ) ) ;
#17966 = VERTEX_POINT ( 'NONE', #4701 ) ;
#17967 = DIRECTION ( 'NONE',  ( 0.000000000000000000, -1.000000000000000000, 0.000000000000000000 ) ) ;
#17968 = ORIENTED_EDGE ( 'NONE', *, *, #5382, .T. ) ;
#17969 = LINE ( 'NONE', #1077, #16604 ) ;
#17970 = CARTESIAN_POINT ( 'NONE',  ( 33.19999999999999574, -84.70000000000001705, 78.50000000000000000 ) ) ;
#17971 = ORIENTED_EDGE ( 'NONE', *, *, #21612, .T. ) ;
#17972 = ORIENTED_EDGE ( 'NONE', *, *, #18276, .F. ) ;
#17973 = CARTESIAN_POINT ( 'NONE',  ( -31.50000000000002132, -71.70000000000001705, 3.200000000000000178 ) ) ;
#17974 = CARTESIAN_POINT ( 'NONE',  ( -31.50000000000002132, 71.00000000000001421, 1.800000000000000044 ) ) ;
#17975 = DIRECTION ( 'NONE',  ( 0.000000000000000000, 0.000000000000000000, -1.000000000000000000 ) ) ;
#17976 = ORIENTED_EDGE ( 'NONE', *, *, #17832, .F. ) ;
#17977 = EDGE_CURVE ( 'NONE', #5468, #21585, #14418, .T. ) ;
#17978 = EDGE_LOOP ( 'NONE', ( #3676, #12952, #21827, #6086, #16170, #2202 ) ) ;
#17979 = DIRECTION ( 'NONE',  ( 0.000000000000000000, 0.000000000000000000, 1.000000000000000000 ) ) ;
#17980 = ORIENTED_EDGE ( 'NONE', *, *, #18049, .F. ) ;
#17981 = DIRECTION ( 'NONE',  ( 3.052134192567367925E-16, 1.000000000000000000, -0.000000000000000000 ) ) ;
#17982 = DIRECTION ( 'NONE',  ( -0.000000000000000000, 1.000000000000000000, 0.000000000000000000 ) ) ;
#17983 = CARTESIAN_POINT ( 'NONE',  ( 9.141460742840918030, -33.43424481021354921, 68.00000000000000000 ) ) ;
#17984 = DIRECTION ( 'NONE',  ( 0.000000000000000000, 0.000000000000000000, 1.000000000000000000 ) ) ;
#17985 = ADVANCED_FACE ( 'NONE', ( #11512 ), #10974, .F. ) ;
#17986 = EDGE_CURVE ( 'NONE', #16569, #9928, #8702, .T. ) ;
#17987 = CARTESIAN_POINT ( 'NONE',  ( -30.49999999999999289, -123.9599366953518711, 0.2999999999999999334 ) ) ;
#17988 = VERTEX_POINT ( 'NONE', #20480 ) ;
#17989 = FACE_OUTER_BOUND ( 'NONE', #14466, .T. ) ;
#17990 = ADVANCED_FACE ( 'NONE', ( #21828 ), #10293, .T. ) ;
#17991 = FACE_OUTER_BOUND ( 'NONE', #5125, .T. ) ;
#17992 = DIRECTION ( 'NONE',  ( -0.000000000000000000, 0.000000000000000000, 1.000000000000000000 ) ) ;
#17993 = LINE ( 'NONE', #1199, #8899 ) ;
#17995 = CIRCLE ( 'NONE', #12631, 0.5000000000000004441 ) ;
#17994 = DIRECTION ( 'NONE',  ( -0.000000000000000000, -1.000000000000000000, 0.000000000000000000 ) ) ;
#17996 = ORIENTED_EDGE ( 'NONE', *, *, #6532, .F. ) ;
#17997 = ORIENTED_EDGE ( 'NONE', *, *, #19738, .F. ) ;
#17998 = DIRECTION ( 'NONE',  ( 0.000000000000000000, 0.000000000000000000, 1.000000000000000000 ) ) ;
#17999 = ADVANCED_FACE ( 'NONE', ( #15090 ), #7412, .F. ) ;
#18000 = CIRCLE ( 'NONE', #15853, 1.750000000000001554 ) ;
#18001 = ORIENTED_EDGE ( 'NONE', *, *, #21477, .F. ) ;
#18002 = VECTOR ( 'NONE', #6908, 1000.000000000000000 ) ;
#18003 = FILL_AREA_STYLE ('',( #11179 ) ) ;
#18004 = ADVANCED_FACE ( 'NONE', ( #5037 ), #4805, .T. ) ;
#18005 = DIRECTION ( 'NONE',  ( 0.000000000000000000, 0.000000000000000000, 1.000000000000000000 ) ) ;
#18006 = ORIENTED_EDGE ( 'NONE', *, *, #3629, .T. ) ;
#18007 = DIRECTION ( 'NONE',  ( -0.000000000000000000, 1.000000000000000000, -0.000000000000000000 ) ) ;
#18008 = ORIENTED_EDGE ( 'NONE', *, *, #1858, .F. ) ;
#18009 = CARTESIAN_POINT ( 'NONE',  ( 29.13662752439705272, -5.299999999999999822, 7.500000000000000000 ) ) ;
#18010 = DIRECTION ( 'NONE',  ( -1.000000000000000000, 0.000000000000000000, 0.000000000000000000 ) ) ;
#18011 = ADVANCED_FACE ( 'NONE', ( #8383 ), #8058, .T. ) ;
#18012 = FACE_OUTER_BOUND ( 'NONE', #14799, .T. ) ;
#18013 = ADVANCED_FACE ( 'NONE', ( #3128 ), #6703, .T. ) ;
#18014 = LINE ( 'NONE', #13083, #1567 ) ;
#18015 = CARTESIAN_POINT ( 'NONE',  ( 27.67540678000427690, 10.94079601157914539, 13.50000000000000000 ) ) ;
#18016 = DIRECTION ( 'NONE',  ( 1.000000000000000000, 0.000000000000000000, 0.000000000000000000 ) ) ;
#18017 = ORIENTED_EDGE ( 'NONE', *, *, #4313, .T. ) ;
#18018 = CARTESIAN_POINT ( 'NONE',  ( 29.37540678000427619, 5.000000000000000000, 7.500000000000000000 ) ) ;
#18019 = CARTESIAN_POINT ( 'NONE',  ( 27.37540678000427619, 5.683640910026986681, 42.50000000000000000 ) ) ;
#18020 = ORIENTED_EDGE ( 'NONE', *, *, #20381, .F. ) ;
#18021 = DIRECTION ( 'NONE',  ( 5.192538640813645496E-17, -1.000000000000000000, -6.359025825921378559E-33 ) ) ;
#18022 =( NAMED_UNIT ( * ) SI_UNIT ( $, .STERADIAN. ) SOLID_ANGLE_UNIT ( ) );
#18023 = EDGE_LOOP ( 'NONE', ( #13490, #15134, #16227, #14510 ) ) ;
#18024 = ORIENTED_EDGE ( 'NONE', *, *, #13295, .T. ) ;
#18025 = EDGE_CURVE ( 'NONE', #21063, #15844, #7758, .T. ) ;
#18026 = EDGE_CURVE ( 'NONE', #15663, #8641, #12057, .T. ) ;
#18027 = EDGE_CURVE ( 'NONE', #9063, #8556, #11316, .T. ) ;
#18028 = CIRCLE ( 'NONE', #9841, 5.300000000000006040 ) ;
#18029 = EDGE_LOOP ( 'NONE', ( #9156, #937, #11435, #15764 ) ) ;
#18030 = DIRECTION ( 'NONE',  ( -1.000000000000000000, 0.000000000000000000, 0.000000000000000000 ) ) ;
#18031 = CARTESIAN_POINT ( 'NONE',  ( -34.39999999999999858, -84.70000000000001705, 5.421010862427522170E-17 ) ) ;
#18032 = VERTEX_POINT ( 'NONE', #1781 ) ;
#18033 = CARTESIAN_POINT ( 'NONE',  ( 18.05178606074127501, -38.87061083372239523, 13.49999999999999822 ) ) ;
#18034 = DIRECTION ( 'NONE',  ( -0.000000000000000000, -0.000000000000000000, -1.000000000000000000 ) ) ;
#18035 = CARTESIAN_POINT ( 'NONE',  ( 15.06741964789885024, 51.94542257242142824, 13.49999999999999645 ) ) ;
#18036 = DIRECTION ( 'NONE',  ( 1.000000000000000000, 0.000000000000000000, 0.000000000000000000 ) ) ;
#18037 = CARTESIAN_POINT ( 'NONE',  ( 27.37540678000427619, 7.754037881813018962E-15, 42.50000000000000000 ) ) ;
#18038 = ORIENTED_EDGE ( 'NONE', *, *, #14394, .T. ) ;
#18039 = DIRECTION ( 'NONE',  ( 0.000000000000000000, 1.000000000000000000, 0.000000000000000000 ) ) ;
#18040 = CARTESIAN_POINT ( 'NONE',  ( -29.13662752439705272, 0.000000000000000000, 13.19999999999999929 ) ) ;
#18041 = ORIENTED_EDGE ( 'NONE', *, *, #446, .F. ) ;
#18042 = ORIENTED_EDGE ( 'NONE', *, *, #8733, .T. ) ;
#18043 = VECTOR ( 'NONE', #94, 1000.000000000000000 ) ;
#18044 = ORIENTED_EDGE ( 'NONE', *, *, #1796, .T. ) ;
#18045 = FACE_OUTER_BOUND ( 'NONE', #20886, .T. ) ;
#18046 = CARTESIAN_POINT ( 'NONE',  ( -8.134906293162368129, 43.00645089659919051, 68.06527860057354928 ) ) ;
#18047 = ORIENTED_EDGE ( 'NONE', *, *, #18176, .T. ) ;
#18048 = DIRECTION ( 'NONE',  ( 0.000000000000000000, -1.000000000000000000, 0.000000000000000000 ) ) ;
#18049 = EDGE_CURVE ( 'NONE', #4799, #14241, #16311, .T. ) ;
#18050 = ORIENTED_EDGE ( 'NONE', *, *, #19215, .F. ) ;
#18051 = DIRECTION ( 'NONE',  ( 1.000000000000000000, 0.000000000000000000, 0.000000000000000000 ) ) ;
#18052 = STYLED_ITEM ( 'NONE', ( #5628 ), #5668 ) ;
#18053 = DIRECTION ( 'NONE',  ( 1.000000000000000000, -0.000000000000000000, 0.000000000000000000 ) ) ;
#18054 = CARTESIAN_POINT ( 'NONE',  ( 9.141460742840918030, -32.11873716947361856, 68.00000000000000000 ) ) ;
#18055 = DIRECTION ( 'NONE',  ( 1.000000000000000000, 0.000000000000000000, 0.000000000000000000 ) ) ;
#18056 = TOROIDAL_SURFACE ( 'NONE', #6302, 5.193574995607837863, 1.000000000000000000 ) ;
#18057 = CARTESIAN_POINT ( 'NONE',  ( 1.724728116533979616, 42.36054587065083155, 51.80876104995653719 ) ) ;
#18058 = VECTOR ( 'NONE', #7227, 1000.000000000000000 ) ;
#18059 = DIRECTION ( 'NONE',  ( 1.000000000000000000, 0.000000000000000000, -0.000000000000000000 ) ) ;
#18060 = VECTOR ( 'NONE', #2417, 1000.000000000000000 ) ;
#18061 = ORIENTED_EDGE ( 'NONE', *, *, #18440, .F. ) ;
#18062 = DIRECTION ( 'NONE',  ( 1.000000000000000000, -0.000000000000000000, -0.000000000000000000 ) ) ;
#18063 = CARTESIAN_POINT ( 'NONE',  ( -23.02398829872514341, -5.683640910026986681, 42.50000000000000000 ) ) ;
#18064 = DIRECTION ( 'NONE',  ( 0.000000000000000000, 0.000000000000000000, 1.000000000000000000 ) ) ;
#18065 = DIRECTION ( 'NONE',  ( 1.000000000000000000, 0.000000000000000000, -0.000000000000000000 ) ) ;
#18066 = VERTEX_POINT ( 'NONE', #8620 ) ;
#18067 = DIRECTION ( 'NONE',  ( -2.107255972849994642E-16, 0.000000000000000000, -1.000000000000000000 ) ) ;
#18068 = DIRECTION ( 'NONE',  ( 0.000000000000000000, 0.000000000000000000, 1.000000000000000000 ) ) ;
#18069 = ORIENTED_EDGE ( 'NONE', *, *, #18957, .T. ) ;
#18070 = DIRECTION ( 'NONE',  ( 0.000000000000000000, -0.000000000000000000, -1.000000000000000000 ) ) ;
#18071 = DIRECTION ( 'NONE',  ( 0.000000000000000000, 0.000000000000000000, 1.000000000000000000 ) ) ;
#18072 = VERTEX_POINT ( 'NONE', #103 ) ;
#18073 = VECTOR ( 'NONE', #3896, 1000.000000000000000 ) ;
#18074 = VECTOR ( 'NONE', #20475, 1000.000000000000000 ) ;
#18075 = AXIS2_PLACEMENT_3D ( 'NONE', #5748, #3946, #12417 ) ;
#18076 = EDGE_LOOP ( 'NONE', ( #3769, #6221, #16796, #17667 ) ) ;
#18077 = DIRECTION ( 'NONE',  ( 0.1868663427273192512, -0.9823853469773029534, 0.000000000000000000 ) ) ;
#18078 = DIRECTION ( 'NONE',  ( -0.000000000000000000, 0.000000000000000000, 1.000000000000000000 ) ) ;
#18079 = CARTESIAN_POINT ( 'NONE',  ( -23.32398829872514057, 2.157133568460765538, 7.500000000000000000 ) ) ;
#18080 = ORIENTED_EDGE ( 'NONE', *, *, #21927, .T. ) ;
#18081 = AXIS2_PLACEMENT_3D ( 'NONE', #18511, #11677, #11898 ) ;
#18082 = EDGE_CURVE ( 'NONE', #12578, #19724, #19923, .T. ) ;
#18083 = ADVANCED_FACE ( 'NONE', ( #16654 ), #20263, .T. ) ;
#18084 = EDGE_LOOP ( 'NONE', ( #13154, #957, #13986, #2517 ) ) ;
#18085 = FACE_OUTER_BOUND ( 'NONE', #13502, .T. ) ;
#18086 = DIRECTION ( 'NONE',  ( -0.000000000000000000, -0.000000000000000000, -1.000000000000000000 ) ) ;
#18087 = LINE ( 'NONE', #6593, #265 ) ;
#18088 = CARTESIAN_POINT ( 'NONE',  ( 34.99999999999999289, 85.00000000000000000, 80.00000000000000000 ) ) ;
#18089 = AXIS2_PLACEMENT_3D ( 'NONE', #2294, #15930, #9242 ) ;
#18090 = VECTOR ( 'NONE', #9697, 1000.000000000000000 ) ;
#18091 = CIRCLE ( 'NONE', #13443, 0.1000000000000028644 ) ;
#18092 = DIRECTION ( 'NONE',  ( 0.000000000000000000, -0.000000000000000000, 1.000000000000000000 ) ) ;
#18093 = CIRCLE ( 'NONE', #10941, 0.2500000000000011657 ) ;
#18094 = DIRECTION ( 'NONE',  ( 0.000000000000000000, 0.000000000000000000, 1.000000000000000000 ) ) ;
#18095 = FACE_OUTER_BOUND ( 'NONE', #17340, .T. ) ;
#18096 = CARTESIAN_POINT ( 'NONE',  ( 9.641460742840918030, 32.61873716947361856, 42.50000000000000711 ) ) ;
#18097 = DIRECTION ( 'NONE',  ( -0.000000000000000000, -0.000000000000000000, -1.000000000000000000 ) ) ;
#18098 = VERTEX_POINT ( 'NONE', #2916 ) ;
#18099 = LINE ( 'NONE', #16533, #13037 ) ;
#18100 = CIRCLE ( 'NONE', #7045, 1.299999999999999156 ) ;
#18101 = EDGE_CURVE ( 'NONE', #18107, #17257, #11687, .T. ) ;
#18102 = CARTESIAN_POINT ( 'NONE',  ( -30.67540678000428045, 63.74634676501045050, 3.500000000000000000 ) ) ;
#18103 = CARTESIAN_POINT ( 'NONE',  ( 15.21174975910705918, 42.31054587065082728, 13.50000000000000000 ) ) ;
#18104 = ORIENTED_EDGE ( 'NONE', *, *, #16346, .F. ) ;
#18105 = LINE ( 'NONE', #9736, #2087 ) ;
#18106 = FACE_OUTER_BOUND ( 'NONE', #18328, .T. ) ;
#18107 = VERTEX_POINT ( 'NONE', #6178 ) ;
#18108 = TOROIDAL_SURFACE ( 'NONE', #14174, 4.051418481279137396, 0.2999999999999999889 ) ;
#18109 = AXIS2_PLACEMENT_3D ( 'NONE', #1444, #11287, #15096 ) ;
#18110 = AXIS2_PLACEMENT_3D ( 'NONE', #1851, #18867, #13920 ) ;
#18111 = EDGE_LOOP ( 'NONE', ( #9661, #15812, #5497, #11759 ) ) ;
#18112 = CYLINDRICAL_SURFACE ( 'NONE', #22128, 0.04999999999999991257 ) ;
#18113 = ADVANCED_FACE ( 'NONE', ( #14990 ), #21507, .F. ) ;
#18114 = EDGE_CURVE ( 'NONE', #8248, #1905, #21725, .T. ) ;
#18115 = VECTOR ( 'NONE', #18612, 1000.000000000000000 ) ;
#18116 = ORIENTED_EDGE ( 'NONE', *, *, #2252, .T. ) ;
#18117 = CARTESIAN_POINT ( 'NONE',  ( -9.141460742840918030, 32.61873716947361856, 42.50000000000000000 ) ) ;
#18118 = ADVANCED_FACE ( 'NONE', ( #6513 ), #13105, .T. ) ;
#18119 = ORIENTED_EDGE ( 'NONE', *, *, #2764, .F. ) ;
#18120 = DIRECTION ( 'NONE',  ( 1.000000000000000000, 0.000000000000000000, 0.000000000000000000 ) ) ;
#18121 = ORIENTED_EDGE ( 'NONE', *, *, #20709, .F. ) ;
#18122 = CARTESIAN_POINT ( 'NONE',  ( -8.134906293162368129, 43.00645089659919051, 68.06527860057354928 ) ) ;
#18123 = LINE ( 'NONE', #9640, #21327 ) ;
#18124 = DIRECTION ( 'NONE',  ( 0.000000000000000000, 1.000000000000000000, 0.000000000000000000 ) ) ;
#18125 = AXIS2_PLACEMENT_3D ( 'NONE', #21694, #20123, #18319 ) ;
#18126 = VECTOR ( 'NONE', #20374, 1000.000000000000000 ) ;
#18127 = DIRECTION ( 'NONE',  ( -0.000000000000000000, -0.000000000000000000, -1.000000000000000000 ) ) ;
#18128 = CYLINDRICAL_SURFACE ( 'NONE', #18995, 0.2500000000000002220 ) ;
#18129 = EDGE_CURVE ( 'NONE', #11579, #5130, #8480, .T. ) ;
#18130 = CARTESIAN_POINT ( 'NONE',  ( 8.641460742840918030, 33.93424481021354921, 68.00000000000000000 ) ) ;
#18131 = AXIS2_PLACEMENT_3D ( 'NONE', #11583, #8253, #20215 ) ;
#18132 = DIRECTION ( 'NONE',  ( 1.000000000000000000, 0.000000000000000000, 0.000000000000000000 ) ) ;
#18133 = FACE_OUTER_BOUND ( 'NONE', #10239, .T. ) ;
#18134 = VECTOR ( 'NONE', #4974, 1000.000000000000000 ) ;
#18135 = VECTOR ( 'NONE', #14552, 1000.000000000000000 ) ;
#18136 = ORIENTED_EDGE ( 'NONE', *, *, #7247, .T. ) ;
#18137 = DIRECTION ( 'NONE',  ( -0.000000000000000000, -0.000000000000000000, -1.000000000000000000 ) ) ;
#18138 = DIRECTION ( 'NONE',  ( -0.000000000000000000, 0.000000000000000000, 1.000000000000000000 ) ) ;
#18139 = ORIENTED_EDGE ( 'NONE', *, *, #17810, .T. ) ;
#18140 = ORIENTED_EDGE ( 'NONE', *, *, #21177, .F. ) ;
#18141 = FACE_OUTER_BOUND ( 'NONE', #17333, .T. ) ;
#18142 = DIRECTION ( 'NONE',  ( 0.000000000000000000, 0.000000000000000000, 1.000000000000000000 ) ) ;
#18143 = EDGE_CURVE ( 'NONE', #18524, #17779, #11518, .T. ) ;
#18144 = VECTOR ( 'NONE', #20890, 1000.000000000000000 ) ;
#18145 = ORIENTED_EDGE ( 'NONE', *, *, #12349, .T. ) ;
#18146 = ADVANCED_FACE ( 'NONE', ( #8183 ), #952, .T. ) ;
#18147 = AXIS2_PLACEMENT_3D ( 'NONE', #11954, #8389, #13738 ) ;
#18148 = VECTOR ( 'NONE', #1132, 1000.000000000000000 ) ;
#18149 = ORIENTED_EDGE ( 'NONE', *, *, #16694, .F. ) ;
#18150 = VECTOR ( 'NONE', #8708, 1000.000000000000000 ) ;
#18151 = CARTESIAN_POINT ( 'NONE',  ( 15.21174975910706095, -52.00603550409435627, 13.50000000000000000 ) ) ;
#18152 = DIRECTION ( 'NONE',  ( -0.000000000000000000, 1.000000000000000000, 0.000000000000000000 ) ) ;
#18153 = ORIENTED_EDGE ( 'NONE', *, *, #6065, .F. ) ;
#18154 = LINE ( 'NONE', #9672, #9294 ) ;
#18155 = DIRECTION ( 'NONE',  ( -0.000000000000000000, -0.000000000000000000, -1.000000000000000000 ) ) ;
#18156 = PLANE ( 'NONE',  #758 ) ;
#18157 = CIRCLE ( 'NONE', #8128, 0.9652499999999990532 ) ;
#18158 = VECTOR ( 'NONE', #745, 1000.000000000000000 ) ;
#18159 = DIRECTION ( 'NONE',  ( -0.000000000000000000, -1.000000000000000000, -0.000000000000000000 ) ) ;
#18160 = EDGE_CURVE ( 'NONE', #15453, #13909, #20641, .T. ) ;
#18161 = ORIENTED_EDGE ( 'NONE', *, *, #16425, .F. ) ;
#18162 = DIRECTION ( 'NONE',  ( -0.000000000000000000, 1.000000000000000000, -0.000000000000000000 ) ) ;
#18163 = CARTESIAN_POINT ( 'NONE',  ( 33.19999999999999574, 85.00000000000000000, 1.500000000000004219 ) ) ;
#18164 = ADVANCED_FACE ( 'NONE', ( #16320 ), #4473, .T. ) ;
#18165 = AXIS2_PLACEMENT_3D ( 'NONE', #12585, #16052, #7582 ) ;
#18166 = ORIENTED_EDGE ( 'NONE', *, *, #2249, .F. ) ;
#18167 = AXIS2_PLACEMENT_3D ( 'NONE', #10119, #13129, #3063 ) ;
#18168 = VERTEX_POINT ( 'NONE', #9847 ) ;
#18169 = VECTOR ( 'NONE', #20831, 1000.000000000000000 ) ;
#18170 = VERTEX_POINT ( 'NONE', #7962 ) ;
#18171 = DIRECTION ( 'NONE',  ( -0.000000000000000000, 0.000000000000000000, 1.000000000000000000 ) ) ;
#18172 = AXIS2_PLACEMENT_3D ( 'NONE', #15187, #9837, #3454 ) ;
#18173 = DIRECTION ( 'NONE',  ( 2.388292521039847891E-16, 0.000000000000000000, 1.000000000000000000 ) ) ;
#18174 = VERTEX_POINT ( 'NONE', #9964 ) ;
#18175 = PLANE ( 'NONE',  #16689 ) ;
#18176 = EDGE_CURVE ( 'NONE', #7001, #6175, #8289, .T. ) ;
#18177 = EDGE_LOOP ( 'NONE', ( #14384, #10247, #18562, #9506 ) ) ;
#18178 = CARTESIAN_POINT ( 'NONE',  ( 4.127054932750481520, -33.43424481021354921, 42.50000000000000000 ) ) ;
#18179 = AXIS2_PLACEMENT_3D ( 'NONE', #19004, #7149, #20471 ) ;
#18180 = DIRECTION ( 'NONE',  ( 0.000000000000000000, 1.000000000000000000, 0.000000000000000000 ) ) ;
#18181 = DIRECTION ( 'NONE',  ( -1.000000000000000000, 0.000000000000000000, 0.000000000000000000 ) ) ;
#18182 = DIRECTION ( 'NONE',  ( 0.000000000000000000, 0.000000000000000000, -1.000000000000000000 ) ) ;
#18183 = AXIS2_PLACEMENT_3D ( 'NONE', #6794, #18297, #4658 ) ;
#18184 = DIRECTION ( 'NONE',  ( 1.000000000000000000, 0.000000000000000000, -0.000000000000000000 ) ) ;
#18185 = CARTESIAN_POINT ( 'NONE',  ( 0.000000000000000000, 4.700000000000000178, 3.799999999999999822 ) ) ;
#18186 = ORIENTED_EDGE ( 'NONE', *, *, #16359, .F. ) ;
#18187 = CARTESIAN_POINT ( 'NONE',  ( 1.824728116533979705, 43.26054587065083012, 29.66679706732590560 ) ) ;
#18188 = CARTESIAN_POINT ( 'NONE',  ( 29.37540678000427619, 6.000000000000000000, 7.500000000000000000 ) ) ;
#18189 = VECTOR ( 'NONE', #5929, 1000.000000000000000 ) ;
#18190 = DIRECTION ( 'NONE',  ( 0.000000000000000000, 0.000000000000000000, -1.000000000000000000 ) ) ;
#18191 = CARTESIAN_POINT ( 'NONE',  ( -1.724728116533986721, 43.31054587065082728, 27.75876104995654003 ) ) ;
#18192 = FACE_OUTER_BOUND ( 'NONE', #7514, .T. ) ;
#18193 = ORIENTED_EDGE ( 'NONE', *, *, #3389, .F. ) ;
#18194 = DIRECTION ( 'NONE',  ( 1.000000000000000000, 0.000000000000000000, 0.000000000000000000 ) ) ;
#18195 = CARTESIAN_POINT ( 'NONE',  ( -33.20000000000000284, -85.00000000000000000, 1.500000000000000000 ) ) ;
#18196 = EDGE_CURVE ( 'NONE', #21163, #14946, #3833, .T. ) ;
#18197 = ORIENTED_EDGE ( 'NONE', *, *, #18292, .F. ) ;
#18198 = LINE ( 'NONE', #12926, #10912 ) ;
#18199 = LINE ( 'NONE', #9258, #7039 ) ;
#18200 = EDGE_CURVE ( 'NONE', #13615, #21066, #4543, .T. ) ;
#18201 = ORIENTED_EDGE ( 'NONE', *, *, #7960, .T. ) ;
#18202 = EDGE_LOOP ( 'NONE', ( #18416, #7721, #9807, #14338 ) ) ;
#18203 = VERTEX_POINT ( 'NONE', #6614 ) ;
#18204 = CARTESIAN_POINT ( 'NONE',  ( -15.04741597961255728, 51.92573430214628871, 13.50000000000006750 ) ) ;
#18205 = DIRECTION ( 'NONE',  ( 1.000000000000000000, 0.000000000000000000, 0.000000000000000000 ) ) ;
#18206 = CARTESIAN_POINT ( 'NONE',  ( -1.724728116533986721, 43.31054587065082728, 43.80876104995653719 ) ) ;
#18207 = AXIS2_PLACEMENT_3D ( 'NONE', #21943, #6620, #6738 ) ;
#18208 = ORIENTED_EDGE ( 'NONE', *, *, #17291, .T. ) ;
#18209 = ORIENTED_EDGE ( 'NONE', *, *, #13664, .T. ) ;
#18210 = CARTESIAN_POINT ( 'NONE',  ( 15.21174975910707161, 41.81054587065082728, 68.50000000000000000 ) ) ;
#18211 = CARTESIAN_POINT ( 'NONE',  ( -14.96174975910705207, -41.81054587065082728, 13.79999999999999893 ) ) ;
#18212 = CARTESIAN_POINT ( 'NONE',  ( -23.10708008847558403, -2.595912616485783975, 13.38952209624200762 ) ) ;
#18213 = DIRECTION ( 'NONE',  ( 0.000000000000000000, -1.000000000000000000, 0.000000000000000000 ) ) ;
#18214 = EDGE_CURVE ( 'NONE', #13600, #20804, #3477, .T. ) ;
#18215 = CYLINDRICAL_SURFACE ( 'NONE', #13904, 3.500000000000003109 ) ;
#18216 = LINE ( 'NONE', #19789, #19731 ) ;
#18217 = LINE ( 'NONE', #9727, #3532 ) ;
#18218 = AXIS2_PLACEMENT_3D ( 'NONE', #2554, #16079, #19561 ) ;
#18219 = AXIS2_PLACEMENT_3D ( 'NONE', #1072, #7920, #11366 ) ;
#18220 = CIRCLE ( 'NONE', #18570, 0.3000000000000016542 ) ;
#18221 = CARTESIAN_POINT ( 'NONE',  ( -8.378839169841052481, 41.92645089659918511, 68.06527860057354928 ) ) ;
#18222 = LINE ( 'NONE', #15081, #17446 ) ;
#18223 = ORIENTED_EDGE ( 'NONE', *, *, #21733, .F. ) ;
#18224 = CARTESIAN_POINT ( 'NONE',  ( 15.95292532278785913, 52.39333383871510108, 13.79999999999999716 ) ) ;
#18225 = EDGE_CURVE ( 'NONE', #8345, #11274, #9636, .T. ) ;
#18226 = ADVANCED_FACE ( 'NONE', ( #12168 ), #10301, .T. ) ;
#18227 = CARTESIAN_POINT ( 'NONE',  ( -1.724728116533986721, 43.31054587065082728, 29.71679706732590631 ) ) ;
#18228 = CARTESIAN_POINT ( 'NONE',  ( 33.19999999999999574, 85.00000000000000000, 78.20000000000000284 ) ) ;
#18229 = ORIENTED_EDGE ( 'NONE', *, *, #6505, .F. ) ;
#18230 = FACE_OUTER_BOUND ( 'NONE', #13003, .T. ) ;
#18231 = FACE_OUTER_BOUND ( 'NONE', #8957, .T. ) ;
#18232 = ORIENTED_EDGE ( 'NONE', *, *, #18554, .T. ) ;
#18233 = ORIENTED_EDGE ( 'NONE', *, *, #19674, .T. ) ;
#18234 = CARTESIAN_POINT ( 'NONE',  ( 27.67540678000427690, -10.94079601157914716, 13.50000000000000000 ) ) ;
#18235 = CIRCLE ( 'NONE', #21109, 0.5000000000000000000 ) ;
#18236 = CIRCLE ( 'NONE', #8960, 0.05000000000000143219 ) ;
#18237 = EDGE_CURVE ( 'NONE', #2211, #252, #2395, .T. ) ;
#18238 = DIRECTION ( 'NONE',  ( 0.000000000000000000, 0.000000000000000000, 1.000000000000000000 ) ) ;
#18239 = DIRECTION ( 'NONE',  ( 0.000000000000000000, 0.000000000000000000, -1.000000000000000000 ) ) ;
#18240 = CYLINDRICAL_SURFACE ( 'NONE', #20608, 0.05000000000000143219 ) ;
#18241 = DIRECTION ( 'NONE',  ( 0.000000000000000000, 0.000000000000000000, -1.000000000000000000 ) ) ;
#18242 = CARTESIAN_POINT ( 'NONE',  ( -1.724728116533986721, 42.31054587065082728, 45.71679706732590631 ) ) ;
#18243 = DIRECTION ( 'NONE',  ( 0.000000000000000000, 0.000000000000000000, 1.000000000000000000 ) ) ;
#18244 = CIRCLE ( 'NONE', #8621, 0.2500000000000002220 ) ;
#18245 = EDGE_CURVE ( 'NONE', #3327, #17367, #19554, .T. ) ;
#18246 = CARTESIAN_POINT ( 'NONE',  ( -34.70000000000001705, 85.00000000000000000, 79.39999999999999147 ) ) ;
#18247 = EDGE_CURVE ( 'NONE', #13733, #2108, #4926, .T. ) ;
#18248 = DIRECTION ( 'NONE',  ( -0.000000000000000000, 0.000000000000000000, -1.000000000000000000 ) ) ;
#18249 = CARTESIAN_POINT ( 'NONE',  ( 25.37540678000427263, -67.54634676501045476, 7.799999999999999822 ) ) ;
#18250 = ORIENTED_EDGE ( 'NONE', *, *, #1446, .T. ) ;
#18251 = CARTESIAN_POINT ( 'NONE',  ( -27.37540678000427619, 5.683640910026986681, 13.79999999999999893 ) ) ;
#18252 = EDGE_LOOP ( 'NONE', ( #11108, #19994, #8994 ) ) ;
#18253 = LINE ( 'NONE', #686, #9888 ) ;
#18254 = CARTESIAN_POINT ( 'NONE',  ( -9.178906393579156386, 42.46645089659917716, 70.50000000000000000 ) ) ;
#18255 = ORIENTED_EDGE ( 'NONE', *, *, #21702, .T. ) ;
#18256 = ORIENTED_EDGE ( 'NONE', *, *, #5270, .T. ) ;
#18257 = CARTESIAN_POINT ( 'NONE',  ( 0.000000000000000000, 43.26054587065083012, 33.71679706732589921 ) ) ;
#18258 = UNCERTAINTY_MEASURE_WITH_UNIT (LENGTH_MEASURE( 1.000000000000000082E-05 ), #13995, 'distance_accuracy_value', 'NONE');
#18259 = EDGE_LOOP ( 'NONE', ( #14236, #2836, #8314, #7150 ) ) ;
#18260 = ORIENTED_EDGE ( 'NONE', *, *, #2961, .F. ) ;
#18261 = EDGE_CURVE ( 'NONE', #13526, #1195, #3352, .T. ) ;
#18262 = ORIENTED_EDGE ( 'NONE', *, *, #2968, .T. ) ;
#18263 = VECTOR ( 'NONE', #10185, 1000.000000000000000 ) ;
#18264 = ORIENTED_EDGE ( 'NONE', *, *, #9356, .T. ) ;
#18265 = CARTESIAN_POINT ( 'NONE',  ( 15.12813070831323969, -51.99253567353609640, 13.49999999999999822 ) ) ;
#18266 = CARTESIAN_POINT ( 'NONE',  ( 1.824728116533979705, 43.31054587065082728, 33.66679706732590915 ) ) ;
#18267 = ORIENTED_EDGE ( 'NONE', *, *, #5227, .T. ) ;
#18268 = DIRECTION ( 'NONE',  ( -0.000000000000000000, -0.000000000000000000, -1.000000000000000000 ) ) ;
#18269 = EDGE_CURVE ( 'NONE', #11899, #18617, #15196, .T. ) ;
#18270 = AXIS2_PLACEMENT_3D ( 'NONE', #20764, #17501, #17935 ) ;
#18271 = CARTESIAN_POINT ( 'NONE',  ( 33.19999999999999574, 84.70000000000001705, 78.50000000000000000 ) ) ;
#18272 = VECTOR ( 'NONE', #17938, 1000.000000000000000 ) ;
#18273 = EDGE_CURVE ( 'NONE', #19672, #2805, #13481, .T. ) ;
#18274 = CARTESIAN_POINT ( 'NONE',  ( 1.774728116533979660, 42.31054587065082728, 37.66679706732590915 ) ) ;
#18275 = CARTESIAN_POINT ( 'NONE',  ( -23.04709339880125185, 2.285361808764050817, 13.25160309052396279 ) ) ;
#18276 = EDGE_CURVE ( 'NONE', #5726, #15087, #9933, .T. ) ;
#18277 = CARTESIAN_POINT ( 'NONE',  ( -23.04273156199908357, 2.261510999192738680, 13.19999999999999929 ) ) ;
#18278 = ORIENTED_EDGE ( 'NONE', *, *, #21020, .F. ) ;
#18279 = EDGE_LOOP ( 'NONE', ( #10225, #7212 ) ) ;
#18280 = EDGE_LOOP ( 'NONE', ( #8559, #9120, #901, #15872 ) ) ;
#18281 = FACE_OUTER_BOUND ( 'NONE', #1232, .T. ) ;
#18282 = LINE ( 'NONE', #13459, #9606 ) ;
#18283 = ORIENTED_EDGE ( 'NONE', *, *, #16800, .F. ) ;
#18284 = AXIS2_PLACEMENT_3D ( 'NONE', #7353, #8919, #12145 ) ;
#18285 = DIRECTION ( 'NONE',  ( 0.000000000000000000, 0.000000000000000000, -1.000000000000000000 ) ) ;
#18286 = AXIS2_PLACEMENT_3D ( 'NONE', #7200, #682, #9085 ) ;
#18287 = VECTOR ( 'NONE', #5845, 1000.000000000000000 ) ;
#18288 = TOROIDAL_SURFACE ( 'NONE', #8659, 0.2500000000000000000, 0.2500000000000000000 ) ;
#18289 = ORIENTED_EDGE ( 'NONE', *, *, #12905, .F. ) ;
#18290 = CARTESIAN_POINT ( 'NONE',  ( -9.178906393579156386, 42.46645089659917716, 68.50000000000000000 ) ) ;
#18291 = DIRECTION ( 'NONE',  ( -0.000000000000000000, 0.000000000000000000, 1.000000000000000000 ) ) ;
#18292 = EDGE_CURVE ( 'NONE', #3127, #13680, #15326, .T. ) ;
#18293 = CARTESIAN_POINT ( 'NONE',  ( -15.95292532278785913, -50.11873716947361856, 68.50000000000000000 ) ) ;
#18294 = CARTESIAN_POINT ( 'NONE',  ( 17.45292532278785913, -34.11873716947361856, 68.50000000000000000 ) ) ;
#18295 = ORIENTED_EDGE ( 'NONE', *, *, #1494, .T. ) ;
#18296 = DIRECTION ( 'NONE',  ( 2.107255972849994642E-16, -0.000000000000000000, 1.000000000000000000 ) ) ;
#18297 = DIRECTION ( 'NONE',  ( 1.000000000000000000, 0.000000000000000000, 0.000000000000000000 ) ) ;
#18298 = CARTESIAN_POINT ( 'NONE',  ( 25.37540678000427263, 68.74634676501045760, 3.799999999999999822 ) ) ;
#18299 = LINE ( 'NONE', #2975, #6188 ) ;
#18300 = ORIENTED_EDGE ( 'NONE', *, *, #2347, .T. ) ;
#18301 = DIRECTION ( 'NONE',  ( 0.000000000000000000, 0.000000000000000000, -1.000000000000000000 ) ) ;
#18302 = DIRECTION ( 'NONE',  ( -0.000000000000000000, -1.000000000000000000, -0.000000000000000000 ) ) ;
#18303 = EDGE_CURVE ( 'NONE', #16466, #15168, #14537, .T. ) ;
#18304 = VECTOR ( 'NONE', #17451, 1000.000000000000114 ) ;
#18305 = EDGE_LOOP ( 'NONE', ( #11443, #11013, #3457, #19267 ) ) ;
#18306 = DIRECTION ( 'NONE',  ( 1.000000000000000000, 0.000000000000000000, 0.000000000000000000 ) ) ;
#18307 = VECTOR ( 'NONE', #13825, 1000.000000000000000 ) ;
#18308 = DIRECTION ( 'NONE',  ( 0.000000000000000000, -1.000000000000000000, 0.000000000000000000 ) ) ;
#18309 = VERTEX_POINT ( 'NONE', #20813 ) ;
#18310 = EDGE_LOOP ( 'NONE', ( #15712, #13720, #11248, #5886 ) ) ;
#18311 = VERTEX_POINT ( 'NONE', #5379 ) ;
#18312 = CARTESIAN_POINT ( 'NONE',  ( -29.37573593128808369, 68.87573593128806237, -5.214931150217776400E-15 ) ) ;
#18313 = DIRECTION ( 'NONE',  ( -0.000000000000000000, 1.000000000000000000, -0.000000000000000000 ) ) ;
#18314 = DIRECTION ( 'NONE',  ( -1.000000000000000000, -0.000000000000000000, 0.000000000000000000 ) ) ;
#18315 = ORIENTED_EDGE ( 'NONE', *, *, #3472, .F. ) ;
#18316 = AXIS2_PLACEMENT_3D ( 'NONE', #5308, #15356, #20409 ) ;
#18317 = ORIENTED_EDGE ( 'NONE', *, *, #21601, .T. ) ;
#18318 = EDGE_CURVE ( 'NONE', #2078, #21878, #22080, .T. ) ;
#18319 = DIRECTION ( 'NONE',  ( 0.000000000000000000, 0.000000000000000000, 1.000000000000000000 ) ) ;
#18320 = DIRECTION ( 'NONE',  ( -0.000000000000000000, 0.000000000000000000, 1.000000000000000000 ) ) ;
#18321 = ADVANCED_FACE ( 'NONE', ( #4796 ), #10630, .T. ) ;
#18322 = CARTESIAN_POINT ( 'NONE',  ( -29.69597781366221412, 26.24124249474150972, 68.50000000000000000 ) ) ;
#18323 = DIRECTION ( 'NONE',  ( 0.000000000000000000, 0.000000000000000000, -1.000000000000000000 ) ) ;
#18324 = ORIENTED_EDGE ( 'NONE', *, *, #6936, .T. ) ;
#18325 = CARTESIAN_POINT ( 'NONE',  ( -28.57540678000427548, 6.494748934539263274, 13.50000000000000000 ) ) ;
#18326 = DIRECTION ( 'NONE',  ( 0.000000000000000000, 1.000000000000000000, 0.000000000000000000 ) ) ;
#18327 = PLANE ( 'NONE',  #13517 ) ;
#18328 = EDGE_LOOP ( 'NONE', ( #2162, #5448, #13107, #18104, #11951, #8091, #3346, #11342 ) ) ;
#18329 = CARTESIAN_POINT ( 'NONE',  ( 1.774728116533979438, 42.36054587065083155, 47.80876104995653719 ) ) ;
#18330 = DIRECTION ( 'NONE',  ( -0.000000000000000000, -1.000000000000000000, -0.000000000000000000 ) ) ;
#18331 = CARTESIAN_POINT ( 'NONE',  ( -15.95292532278785913, -51.61873716947361856, 68.50000000000000000 ) ) ;
#18332 = EDGE_LOOP ( 'NONE', ( #20114, #14303, #14048, #14550 ) ) ;
#18333 = FACE_OUTER_BOUND ( 'NONE', #4703, .T. ) ;
#18334 = CARTESIAN_POINT ( 'NONE',  ( -33.20000000000001705, 84.70000000000001705, 78.79999999999999716 ) ) ;
#18335 = ORIENTED_EDGE ( 'NONE', *, *, #7176, .T. ) ;
#18336 = EDGE_CURVE ( 'NONE', #17454, #1239, #18790, .T. ) ;
#18337 = ORIENTED_EDGE ( 'NONE', *, *, #16448, .T. ) ;
#18338 = CARTESIAN_POINT ( 'NONE',  ( 29.48732456384755807, -2.488184534793062674, 0.2032168635956394243 ) ) ;
#18339 = ORIENTED_EDGE ( 'NONE', *, *, #17159, .T. ) ;
#18340 = EDGE_CURVE ( 'NONE', #21627, #14858, #11335, .T. ) ;
#18341 = CARTESIAN_POINT ( 'NONE',  ( -9.718906393579157310, 43.26651812033729527, 68.06527860057354928 ) ) ;
#18342 = DIRECTION ( 'NONE',  ( -0.000000000000000000, -0.000000000000000000, -1.000000000000000000 ) ) ;
#18343 = AXIS2_PLACEMENT_3D ( 'NONE', #9869, #11638, #11433 ) ;
#18344 = DIRECTION ( 'NONE',  ( 0.000000000000000000, 1.000000000000000000, 0.000000000000000000 ) ) ;
#18345 = CARTESIAN_POINT ( 'NONE',  ( -34.39999999999999858, 84.70000000000001705, 0.6000000000000033085 ) ) ;
#18346 = CARTESIAN_POINT ( 'NONE',  ( 23.05999184077136377, 2.354728237135330637, 13.30000967910994092 ) ) ;
#18347 = DIRECTION ( 'NONE',  ( 0.000000000000000000, 0.000000000000000000, -1.000000000000000000 ) ) ;
#18348 = CARTESIAN_POINT ( 'NONE',  ( 1.724728116533979616, 43.31054587065082728, 47.80876104995653719 ) ) ;
#18349 = CARTESIAN_POINT ( 'NONE',  ( -14.96174975910705207, -51.83071861726173779, 13.82019355104894309 ) ) ;
#18350 = DIRECTION ( 'NONE',  ( 0.000000000000000000, 0.000000000000000000, -1.000000000000000000 ) ) ;
#18351 = EDGE_CURVE ( 'NONE', #8285, #22005, #4563, .T. ) ;
#18352 = ORIENTED_EDGE ( 'NONE', *, *, #13295, .F. ) ;
#18353 = LINE ( 'NONE', #15005, #5976 ) ;
#18354 = ORIENTED_EDGE ( 'NONE', *, *, #2249, .T. ) ;
#18355 = CARTESIAN_POINT ( 'NONE',  ( 1.724728116533979616, 43.31054587065082728, 39.80876104995653719 ) ) ;
#18356 = CIRCLE ( 'NONE', #7649, 0.05000000000000143219 ) ;
#18357 = AXIS2_PLACEMENT_3D ( 'NONE', #5291, #7185, #15661 ) ;
#18358 = CARTESIAN_POINT ( 'NONE',  ( -33.80000000000000426, -84.70000000000001705, -5.863365348801607979E-15 ) ) ;
#18359 = ORIENTED_EDGE ( 'NONE', *, *, #4624, .F. ) ;
#18360 = ORIENTED_EDGE ( 'NONE', *, *, #18558, .T. ) ;
#18361 = DIRECTION ( 'NONE',  ( 0.000000000000000000, 0.000000000000000000, 1.000000000000000000 ) ) ;
#18362 = DIRECTION ( 'NONE',  ( 0.000000000000000000, 0.000000000000000000, 1.000000000000000000 ) ) ;
#18363 = ORIENTED_EDGE ( 'NONE', *, *, #15510, .F. ) ;
#18364 = ORIENTED_EDGE ( 'NONE', *, *, #8479, .T. ) ;
#18365 = ADVANCED_FACE ( 'NONE', ( #15434 ), #7428, .T. ) ;
#18366 = ORIENTED_EDGE ( 'NONE', *, *, #8597, .T. ) ;
#18367 = ADVANCED_FACE ( 'NONE', ( #5043 ), #19939, .T. ) ;
#18368 = VERTEX_POINT ( 'NONE', #6043 ) ;
#18369 = CARTESIAN_POINT ( 'NONE',  ( -33.20000000000000284, 84.70000000000001705, 1.500000000000000222 ) ) ;
#18370 = DIRECTION ( 'NONE',  ( 1.000000000000000000, 0.000000000000000000, 0.000000000000000000 ) ) ;
#18371 = ORIENTED_EDGE ( 'NONE', *, *, #6402, .F. ) ;
#18372 = LINE ( 'NONE', #9884, #11076 ) ;
#18373 = FACE_OUTER_BOUND ( 'NONE', #11706, .T. ) ;
#18374 = CARTESIAN_POINT ( 'NONE',  ( 1.724728116533978728, 43.31054587065082728, 33.71679706732589921 ) ) ;
#18375 = DIRECTION ( 'NONE',  ( -0.000000000000000000, -0.000000000000000000, -1.000000000000000000 ) ) ;
#18376 = EDGE_CURVE ( 'NONE', #21328, #18168, #15270, .T. ) ;
#18377 = DIRECTION ( 'NONE',  ( 0.000000000000000000, 0.000000000000000000, 1.000000000000000000 ) ) ;
#18378 = EDGE_LOOP ( 'NONE', ( #18954, #4140, #639, #19045 ) ) ;
#18379 = EDGE_LOOP ( 'NONE', ( #5813, #301, #6696, #14412 ) ) ;
#18380 = ORIENTED_EDGE ( 'NONE', *, *, #6517, .T. ) ;
#18381 = DIRECTION ( 'NONE',  ( 1.000000000000000000, 0.000000000000000000, 0.000000000000000000 ) ) ;
#18382 = DIRECTION ( 'NONE',  ( 0.000000000000000000, 1.000000000000000000, 0.000000000000000000 ) ) ;
#18383 = VERTEX_POINT ( 'NONE', #7271 ) ;
#18384 = CARTESIAN_POINT ( 'NONE',  ( -1.824728116533986810, 42.36054587065083155, 27.70876104995653577 ) ) ;
#18385 = ADVANCED_FACE ( 'NONE', ( #14501 ), #5594, .F. ) ;
#18386 = ADVANCED_FACE ( 'NONE', ( #21249 ), #9272, .T. ) ;
#18387 = PRODUCT_DEFINITION_SHAPE ( 'NONE', 'NONE',  #22164 ) ;
#18388 = ORIENTED_EDGE ( 'NONE', *, *, #6468, .T. ) ;
#18389 = CARTESIAN_POINT ( 'NONE',  ( 25.37540678000427263, -66.94634676501046044, 13.50000000000000000 ) ) ;
#18390 = DIRECTION ( 'NONE',  ( 0.000000000000000000, 0.000000000000000000, 1.000000000000000000 ) ) ;
#18391 = ADVANCED_FACE ( 'NONE', ( #16077 ), #4024, .T. ) ;
#18392 = CARTESIAN_POINT ( 'NONE',  ( 23.02398829872515051, -3.003070052962832026, 13.75712488064577599 ) ) ;
#18393 = CARTESIAN_POINT ( 'NONE',  ( 30.07540678000427548, 0.000000000000000000, 7.200000000000000178 ) ) ;
#18394 = ORIENTED_EDGE ( 'NONE', *, *, #10924, .T. ) ;
#18395 = CARTESIAN_POINT ( 'NONE',  ( -27.37540678000427619, 5.683640910026986681, 42.50000000000000000 ) ) ;
#18396 = LINE ( 'NONE', #5099, #20341 ) ;
#18397 = CARTESIAN_POINT ( 'NONE',  ( 30.19999999999999574, 70.00000000000000000, 1.200000000000003064 ) ) ;
#18398 = DIRECTION ( 'NONE',  ( 0.9729678061520319332, 0.2309407893632090258, -0.000000000000000000 ) ) ;
#18399 = ORIENTED_EDGE ( 'NONE', *, *, #16909, .T. ) ;
#18400 = CIRCLE ( 'NONE', #21638, 3.800000000000004707 ) ;
#18401 = AXIS2_PLACEMENT_3D ( 'NONE', #12590, #10823, #2309 ) ;
#18402 = EDGE_CURVE ( 'NONE', #2136, #8457, #10619, .T. ) ;
#18403 = ORIENTED_EDGE ( 'NONE', *, *, #9201, .F. ) ;
#18404 = CARTESIAN_POINT ( 'NONE',  ( -8.638906393579159015, 43.51045099701597962, 68.06527860057354928 ) ) ;
#18405 = LINE ( 'NONE', #10252, #18825 ) ;
#18406 = VERTEX_POINT ( 'NONE', #5720 ) ;
#18407 = ORIENTED_EDGE ( 'NONE', *, *, #21287, .T. ) ;
#18408 = ORIENTED_EDGE ( 'NONE', *, *, #8567, .F. ) ;
#18409 = CARTESIAN_POINT ( 'NONE',  ( 1.824728116533979705, 43.31054587065082728, 53.66679706732590915 ) ) ;
#18410 = DIRECTION ( 'NONE',  ( -0.000000000000000000, -1.000000000000000000, -0.000000000000000000 ) ) ;
#18411 = CARTESIAN_POINT ( 'NONE',  ( 1.724728116533979616, 43.26054587065083012, 35.70876104995653577 ) ) ;
#18412 = VERTEX_POINT ( 'NONE', #15852 ) ;
#18413 = DIRECTION ( 'NONE',  ( 0.000000000000000000, -1.000000000000000000, 0.000000000000000000 ) ) ;
#18414 = ORIENTED_EDGE ( 'NONE', *, *, #13185, .T. ) ;
#18415 = EDGE_CURVE ( 'NONE', #2490, #8846, #16181, .T. ) ;
#18416 = ORIENTED_EDGE ( 'NONE', *, *, #4866, .T. ) ;
#18417 = DIRECTION ( 'NONE',  ( 0.000000000000000000, 1.000000000000000000, 0.000000000000000000 ) ) ;
#18418 = CIRCLE ( 'NONE', #8410, 0.05000000000000143219 ) ;
#18419 = AXIS2_PLACEMENT_3D ( 'NONE', #14450, #813, #2846 ) ;
#18420 = AXIS2_PLACEMENT_3D ( 'NONE', #2969, #4320, #11566 ) ;
#18421 = EDGE_CURVE ( 'NONE', #12433, #19117, #7603, .T. ) ;
#18422 = LINE ( 'NONE', #4565, #12395 ) ;
#18423 = DIRECTION ( 'NONE',  ( -0.000000000000000000, -1.000000000000000000, 0.000000000000000000 ) ) ;
#18424 = CARTESIAN_POINT ( 'NONE',  ( -15.95292532278785913, 32.61873716947361856, 68.00000000000000000 ) ) ;
#18425 = DIRECTION ( 'NONE',  ( 0.000000000000000000, -0.000000000000000000, 1.000000000000000000 ) ) ;
#18426 = CARTESIAN_POINT ( 'NONE',  ( -4.127054932750482408, -32.93424481021354921, 68.00000000000000000 ) ) ;
#18427 = ORIENTED_EDGE ( 'NONE', *, *, #12875, .T. ) ;
#18428 = LINE ( 'NONE', #3110, #19595 ) ;
#18429 = CARTESIAN_POINT ( 'NONE',  ( 1.724728116533979616, 43.26054587065083012, 51.70876104995653577 ) ) ;
#18430 = CARTESIAN_POINT ( 'NONE',  ( 30.49999999999999645, -123.9599366953518711, 10.00000000000000178 ) ) ;
#18431 = EDGE_LOOP ( 'NONE', ( #6230, #3880, #1347, #5761 ) ) ;
#18432 = VECTOR ( 'NONE', #14377, 1000.000000000000000 ) ;
#18433 = DIRECTION ( 'NONE',  ( -0.000000000000000000, 1.000000000000000000, -0.000000000000000000 ) ) ;
#18434 = TOROIDAL_SURFACE ( 'NONE', #7729, 1.300000000000000044, 0.2999999999999999889 ) ;
#18435 = DIRECTION ( 'NONE',  ( 0.000000000000000000, 0.000000000000000000, -1.000000000000000000 ) ) ;
#18436 = EDGE_LOOP ( 'NONE', ( #17422, #610, #4848, #21660 ) ) ;
#18437 = CIRCLE ( 'NONE', #551, 6.500000000000002665 ) ;
#18438 = AXIS2_PLACEMENT_3D ( 'NONE', #4290, #16231, #16129 ) ;
#18439 = DIRECTION ( 'NONE',  ( 1.000000000000000000, 0.000000000000000000, 0.000000000000000000 ) ) ;
#18440 = EDGE_CURVE ( 'NONE', #14293, #16984, #14296, .T. ) ;
#18441 = CARTESIAN_POINT ( 'NONE',  ( 15.21174975910707161, 51.61873716947361856, 68.50000000000000000 ) ) ;
#18442 = VERTEX_POINT ( 'NONE', #5917 ) ;
#18443 = EDGE_CURVE ( 'NONE', #12289, #16645, #9157, .T. ) ;
#18444 = ORIENTED_EDGE ( 'NONE', *, *, #5290, .F. ) ;
#18445 = DIRECTION ( 'NONE',  ( 1.000000000000000000, 0.000000000000000000, 6.123233995736764803E-17 ) ) ;
#18446 = CONTEXT_DEPENDENT_SHAPE_REPRESENTATION ( #21464, #20027 ) ;
#18447 = VERTEX_POINT ( 'NONE', #19444 ) ;
#18448 = AXIS2_PLACEMENT_3D ( 'NONE', #886, #5851, #19815 ) ;
#18449 = CIRCLE ( 'NONE', #17744, 0.3000000000000003775 ) ;
#18450 = AXIS2_PLACEMENT_3D ( 'NONE', #4928, #11617, #9748 ) ;
#18451 = CARTESIAN_POINT ( 'NONE',  ( -1.836970198721029934E-16, -72.00000000000001421, 1.800000000000000044 ) ) ;
#18452 = CARTESIAN_POINT ( 'NONE',  ( 30.19999999999999574, 69.70000000000000284, 4.011548038196366406E-15 ) ) ;
#18453 = VECTOR ( 'NONE', #18583, 1000.000000000000000 ) ;
#18454 = CARTESIAN_POINT ( 'NONE',  ( 28.87540678000427619, -6.494748934539263274, 13.50000000000000000 ) ) ;
#18455 = CARTESIAN_POINT ( 'NONE',  ( 1.774728116533973665, 43.26054587065083012, 24.00000000000000000 ) ) ;
#18456 = LINE ( 'NONE', #13417, #10000 ) ;
#18457 = FACE_OUTER_BOUND ( 'NONE', #8595, .T. ) ;
#18458 = CARTESIAN_POINT ( 'NONE',  ( -23.32398829872514057, -5.683640910026986681, 13.79999999999999893 ) ) ;
#18459 = DIRECTION ( 'NONE',  ( 1.000000000000000000, 0.000000000000000000, 0.000000000000000000 ) ) ;
#18460 = AXIS2_PLACEMENT_3D ( 'NONE', #18620, #15144, #13903 ) ;
#18461 = DIRECTION ( 'NONE',  ( -0.000000000000000000, -0.000000000000000000, -1.000000000000000000 ) ) ;
#18462 = CIRCLE ( 'NONE', #7053, 0.6000000000000000888 ) ;
#18463 = AXIS2_PLACEMENT_3D ( 'NONE', #380, #5549, #20770 ) ;
#18464 = ORIENTED_EDGE ( 'NONE', *, *, #19201, .T. ) ;
#18465 = AXIS2_PLACEMENT_3D ( 'NONE', #7836, #1097, #21596 ) ;
#18466 = DIRECTION ( 'NONE',  ( 0.000000000000000000, -1.000000000000000000, 0.000000000000000000 ) ) ;
#18467 = VERTEX_POINT ( 'NONE', #15962 ) ;
#18468 = CARTESIAN_POINT ( 'NONE',  ( 29.20000000000002061, 68.70000000000001705, 0.000000000000000000 ) ) ;
#18469 = EDGE_CURVE ( 'NONE', #1150, #21455, #10290, .T. ) ;
#18470 = VERTEX_POINT ( 'NONE', #21363 ) ;
#18471 = VECTOR ( 'NONE', #6920, 1000.000000000000000 ) ;
#18472 = ORIENTED_EDGE ( 'NONE', *, *, #20217, .F. ) ;
#18473 = DIRECTION ( 'NONE',  ( 0.000000000000000000, 0.000000000000000000, -1.000000000000000000 ) ) ;
#18474 = ORIENTED_EDGE ( 'NONE', *, *, #149, .F. ) ;
#18475 = LINE ( 'NONE', #14672, #12483 ) ;
#18476 = VERTEX_POINT ( 'NONE', #12827 ) ;
#18477 = VERTEX_POINT ( 'NONE', #5821 ) ;
#18478 = VECTOR ( 'NONE', #5259, 1000.000000000000000 ) ;
#18479 = CIRCLE ( 'NONE', #11688, 0.2500000000000002220 ) ;
#18480 = ORIENTED_EDGE ( 'NONE', *, *, #8859, .T. ) ;
#18481 = CARTESIAN_POINT ( 'NONE',  ( 14.96174975910705740, -51.76873716947361004, 13.50000000000000000 ) ) ;
#18482 = AXIS2_PLACEMENT_3D ( 'NONE', #18758, #166, #11704 ) ;
#18483 = EDGE_CURVE ( 'NONE', #9288, #21031, #12705, .T. ) ;
#18484 = CARTESIAN_POINT ( 'NONE',  ( 30.07540678000427548, -63.74634676501045050, 7.500000000000000000 ) ) ;
#18485 = CIRCLE ( 'NONE', #22088, 0.2999999999999999334 ) ;
#18486 = ORIENTED_EDGE ( 'NONE', *, *, #13912, .T. ) ;
#18487 = TOROIDAL_SURFACE ( 'NONE', #3132, 0.05000000000000000278, 0.05000000000000000278 ) ;
#18488 = CYLINDRICAL_SURFACE ( 'NONE', #18316, 0.3000000000000016542 ) ;
#18489 = DIRECTION ( 'NONE',  ( 0.000000000000000000, 1.000000000000000000, 0.000000000000000000 ) ) ;
#18490 = FACE_OUTER_BOUND ( 'NONE', #16169, .T. ) ;
#18491 = ADVANCED_FACE ( 'NONE', ( #17438 ), #4240, .T. ) ;
#18492 = EDGE_CURVE ( 'NONE', #1639, #2728, #9823, .T. ) ;
#18493 = LINE ( 'NONE', #8762, #2558 ) ;
#18494 = ORIENTED_EDGE ( 'NONE', *, *, #1809, .T. ) ;
#18495 = AXIS2_PLACEMENT_3D ( 'NONE', #1635, #10485, #18994 ) ;
#18496 = AXIS2_PLACEMENT_3D ( 'NONE', #4800, #5257, #13402 ) ;
#18497 = ORIENTED_EDGE ( 'NONE', *, *, #9592, .F. ) ;
#18498 = ORIENTED_EDGE ( 'NONE', *, *, #9018, .T. ) ;
#18499 = LINE ( 'NONE', #3396, #18115 ) ;
#18500 = ORIENTED_EDGE ( 'NONE', *, *, #8101, .T. ) ;
#18501 = AXIS2_PLACEMENT_3D ( 'NONE', #1992, #10412, #4028 ) ;
#18502 = DIRECTION ( 'NONE',  ( 0.000000000000000000, 0.000000000000000000, 1.000000000000000000 ) ) ;
#18503 = AXIS2_PLACEMENT_3D ( 'NONE', #2260, #12308, #19165 ) ;
#18504 = CIRCLE ( 'NONE', #11015, 0.04999999999999991257 ) ;
#18505 = ORIENTED_EDGE ( 'NONE', *, *, #20023, .T. ) ;
#18506 = CARTESIAN_POINT ( 'NONE',  ( -3.127054932750481964, 32.61873716947361856, 42.50000000000000711 ) ) ;
#18507 = EDGE_CURVE ( 'NONE', #8501, #15453, #14840, .T. ) ;
#18508 = CARTESIAN_POINT ( 'NONE',  ( -26.56227312273159313, 9.958410664601840878, 13.79999999999999893 ) ) ;
#18509 = AXIS2_PLACEMENT_3D ( 'NONE', #19526, #5794, #10813 ) ;
#18510 = AXIS2_PLACEMENT_3D ( 'NONE', #15461, #1366, #17025 ) ;
#18511 = CARTESIAN_POINT ( 'NONE',  ( -17.45292532278785913, -50.11873716947361856, 14.00000000000000000 ) ) ;
#18512 = ORIENTED_EDGE ( 'NONE', *, *, #10452, .F. ) ;
#18513 = CYLINDRICAL_SURFACE ( 'NONE', #17743, 0.5000000000000004441 ) ;
#18514 = DIRECTION ( 'NONE',  ( 0.000000000000000000, 0.000000000000000000, -1.000000000000000000 ) ) ;
#18515 = CARTESIAN_POINT ( 'NONE',  ( 9.141460742840918030, 32.61873716947361856, 68.00000000000000000 ) ) ;
#18516 = AXIS2_PLACEMENT_3D ( 'NONE', #12807, #6127, #13016 ) ;
#18517 = CARTESIAN_POINT ( 'NONE',  ( -1.774728116533986766, 43.26054587065083012, 12.00000000000000000 ) ) ;
#18518 = EDGE_LOOP ( 'NONE', ( #9711, #19726, #17344, #18863 ) ) ;
#18519 = CARTESIAN_POINT ( 'NONE',  ( 1.724728116533979616, 43.31054587065082728, 27.75876104995653648 ) ) ;
#18520 = TOROIDAL_SURFACE ( 'NONE', #4237, 0.05000000000000000278, 0.05000000000000000278 ) ;
#18521 = AXIS2_PLACEMENT_3D ( 'NONE', #10287, #13519, #13297 ) ;
#18522 = ADVANCED_FACE ( 'NONE', ( #9937 ), #9481, .T. ) ;
#18523 = EDGE_CURVE ( 'NONE', #2320, #8961, #21695, .T. ) ;
#18524 = VERTEX_POINT ( 'NONE', #1418 ) ;
#18525 = CARTESIAN_POINT ( 'NONE',  ( 1.824728116533979705, 43.26054587065083012, 29.66679706732590560 ) ) ;
#18526 = ADVANCED_FACE ( 'NONE', ( #2773 ), #11589, .T. ) ;
#18527 = DIRECTION ( 'NONE',  ( -0.000000000000000000, 0.000000000000000000, 1.000000000000000000 ) ) ;
#18528 = EDGE_LOOP ( 'NONE', ( #16401, #16928, #4177, #8744 ) ) ;
#18529 = ORIENTED_EDGE ( 'NONE', *, *, #7259, .T. ) ;
#18530 = ORIENTED_EDGE ( 'NONE', *, *, #16563, .T. ) ;
#18531 = DIRECTION ( 'NONE',  ( 0.000000000000000000, 0.000000000000000000, 1.000000000000000000 ) ) ;
#18532 = ADVANCED_FACE ( 'NONE', ( #1090 ), #8260, .T. ) ;
#18533 = CARTESIAN_POINT ( 'NONE',  ( -9.641460742840918030, -32.61873716947361856, 68.00000000000000000 ) ) ;
#18534 = VECTOR ( 'NONE', #10716, 1000.000000000000000 ) ;
#18535 = ORIENTED_EDGE ( 'NONE', *, *, #7835, .T. ) ;
#18536 = FACE_OUTER_BOUND ( 'NONE', #10343, .T. ) ;
#18537 = ORIENTED_EDGE ( 'NONE', *, *, #13225, .F. ) ;
#18538 = VECTOR ( 'NONE', #15482, 1000.000000000000000 ) ;
#18539 = ORIENTED_EDGE ( 'NONE', *, *, #3389, .T. ) ;
#18540 = DIRECTION ( 'NONE',  ( -0.000000000000000000, -3.614007241618412274E-15, -1.000000000000000000 ) ) ;
#18541 = TOROIDAL_SURFACE ( 'NONE', #7122, 4.700000000000000178, 0.2999999999999999889 ) ;
#18542 = EDGE_CURVE ( 'NONE', #17755, #6365, #2770, .T. ) ;
#18543 = DIRECTION ( 'NONE',  ( 1.000000000000000000, 0.000000000000000000, 0.000000000000000000 ) ) ;
#18544 = LINE ( 'NONE', #17191, #8861 ) ;
#18545 = DIRECTION ( 'NONE',  ( 1.000000000000000000, 0.000000000000000000, -0.000000000000000000 ) ) ;
#18546 = DIRECTION ( 'NONE',  ( 1.000000000000000000, 0.000000000000000000, 0.000000000000000000 ) ) ;
#18547 = CARTESIAN_POINT ( 'NONE',  ( -23.02398829872513986, 7.027230193580998154E-15, 7.500000000000000000 ) ) ;
#18548 = DIRECTION ( 'NONE',  ( -0.000000000000000000, -1.000000000000000000, -0.000000000000000000 ) ) ;
#18549 = CYLINDRICAL_SURFACE ( 'NONE', #3479, 1.000000000000000888 ) ;
#18550 = SPHERICAL_SURFACE ( 'NONE', #13876, 0.5000000000000000000 ) ;
#18551 = ORIENTED_EDGE ( 'NONE', *, *, #11822, .T. ) ;
#18552 = CYLINDRICAL_SURFACE ( 'NONE', #12664, 0.2500000000000002220 ) ;
#18553 = AXIS2_PLACEMENT_3D ( 'NONE', #16615, #3093, #13273 ) ;
#18554 = EDGE_CURVE ( 'NONE', #16569, #17318, #18087, .T. ) ;
#18555 = DIRECTION ( 'NONE',  ( -0.000000000000000000, -0.000000000000000000, -1.000000000000000000 ) ) ;
#18556 =( BOUNDED_CURVE ( )  B_SPLINE_CURVE ( 3, ( #17612, #20874, #15392, #6916 ),
 .UNSPECIFIED., .F., .T. ) 
 B_SPLINE_CURVE_WITH_KNOTS ( ( 4, 4 ),
 ( 3.141592653589793116, 4.712388980384689674 ),
 .UNSPECIFIED. ) 
 CURVE ( )  GEOMETRIC_REPRESENTATION_ITEM ( )  RATIONAL_B_SPLINE_CURVE ( ( 1.000000000000000000, 0.8047378541243649375, 0.8047378541243649375, 1.000000000000000000 ) ) 
 REPRESENTATION_ITEM ( '' )  );
#18557 = ORIENTED_EDGE ( 'NONE', *, *, #20528, .T. ) ;
#18558 = EDGE_CURVE ( 'NONE', #4102, #13748, #8150, .T. ) ;
#18559 = AXIS2_PLACEMENT_3D ( 'NONE', #14188, #20599, #14079 ) ;
#18560 = DIRECTION ( 'NONE',  ( 1.301042606982568087E-14, 0.000000000000000000, 1.000000000000000000 ) ) ;
#18561 = ORIENTED_EDGE ( 'NONE', *, *, #11172, .T. ) ;
#18562 = ORIENTED_EDGE ( 'NONE', *, *, #21419, .F. ) ;
#18563 = CARTESIAN_POINT ( 'NONE',  ( 15.21174975910705918, -52.10286008774954780, 13.87500000000000000 ) ) ;
#18564 = ORIENTED_EDGE ( 'NONE', *, *, #13946, .F. ) ;
#18565 = VECTOR ( 'NONE', #155, 1000.000000000000000 ) ;
#18566 = CARTESIAN_POINT ( 'NONE',  ( -3.627054932750481964, 32.11873716947361856, 68.00000000000000000 ) ) ;
#18567 = EDGE_LOOP ( 'NONE', ( #14561, #2094, #16118, #19106 ) ) ;
#18568 = DIRECTION ( 'NONE',  ( 1.000000000000000000, -0.000000000000000000, 1.734723475976806848E-16 ) ) ;
#18569 =( GEOMETRIC_REPRESENTATION_CONTEXT ( 3 ) GLOBAL_UNCERTAINTY_ASSIGNED_CONTEXT ( ( #14891 ) ) GLOBAL_UNIT_ASSIGNED_CONTEXT ( ( #19957, #2939, #15016 ) ) REPRESENTATION_CONTEXT ( 'NONE', 'WORKASPACE' ) );
#18570 = AXIS2_PLACEMENT_3D ( 'NONE', #13494, #20334, #5680 ) ;
#18571 = CARTESIAN_POINT ( 'NONE',  ( -8.641460742840918030, -33.43424481021354921, 42.50000000000000000 ) ) ;
#18572 = EDGE_CURVE ( 'NONE', #104, #11610, #6372, .T. ) ;
#18573 = CARTESIAN_POINT ( 'NONE',  ( -1.724728116533986721, 43.31054587065082728, 51.70876104995653577 ) ) ;
#18574 = DIRECTION ( 'NONE',  ( 0.000000000000000000, -1.000000000000000000, 0.000000000000000000 ) ) ;
#18575 = DIRECTION ( 'NONE',  ( 1.000000000000000000, 0.000000000000000000, 0.000000000000000000 ) ) ;
#18576 = DIRECTION ( 'NONE',  ( -0.000000000000000000, -0.000000000000000000, -1.000000000000000000 ) ) ;
#18577 = LINE ( 'NONE', #3028, #18660 ) ;
#18578 = DIRECTION ( 'NONE',  ( 0.000000000000000000, 0.000000000000000000, 1.000000000000000000 ) ) ;
#18579 = ADVANCED_FACE ( 'NONE', ( #16288 ), #14687, .F. ) ;
#18580 = VECTOR ( 'NONE', #11460, 1000.000000000000000 ) ;
#18581 = LINE ( 'NONE', #1898, #13106 ) ;
#18582 = ORIENTED_EDGE ( 'NONE', *, *, #18835, .F. ) ;
#18583 = DIRECTION ( 'NONE',  ( -1.000000000000000000, 0.000000000000000000, 0.000000000000000000 ) ) ;
#18584 = AXIS2_PLACEMENT_3D ( 'NONE', #17093, #16751, #2997 ) ;
#18585 = AXIS2_PLACEMENT_3D ( 'NONE', #13115, #16476, #914 ) ;
#18586 = VERTEX_POINT ( 'NONE', #10384 ) ;
#18587 = ORIENTED_EDGE ( 'NONE', *, *, #4959, .T. ) ;
#18588 = DIRECTION ( 'NONE',  ( 0.000000000000000000, -0.000000000000000000, -1.000000000000000000 ) ) ;
#18589 = SHAPE_REPRESENTATION_RELATIONSHIP ( 'NONE' , 'NONE' ,  #7461, #20354 ) ;
#18590 = VERTEX_POINT ( 'NONE', #8600 ) ;
#18591 =( NAMED_UNIT ( * ) PLANE_ANGLE_UNIT ( ) SI_UNIT ( $, .RADIAN. ) );
#18592 = EDGE_LOOP ( 'NONE', ( #10064, #5942, #18816, #19690 ) ) ;
#18593 = ORIENTED_EDGE ( 'NONE', *, *, #4892, .T. ) ;
#18594 = ORIENTED_EDGE ( 'NONE', *, *, #11341, .T. ) ;
#18595 = CIRCLE ( 'NONE', #2158, 0.2999999999999999334 ) ;
#18596 = EDGE_CURVE ( 'NONE', #7145, #4059, #12762, .T. ) ;
#18597 = CARTESIAN_POINT ( 'NONE',  ( -1.724728116533986721, 43.31054587065082728, 37.66679706732590915 ) ) ;
#18598 = DIRECTION ( 'NONE',  ( -0.000000000000000000, 1.000000000000000000, -0.000000000000000000 ) ) ;
#18599 = STYLED_ITEM ( 'NONE', ( #10538 ), #20594 ) ;
#18600 = ADVANCED_FACE ( 'NONE', ( #13710 ), #616, .F. ) ;
#18601 = DIRECTION ( 'NONE',  ( -1.000000000000000000, -0.000000000000000000, -0.000000000000000000 ) ) ;
#18602 = VERTEX_POINT ( 'NONE', #287 ) ;
#18603 = DIRECTION ( 'NONE',  ( -1.000000000000000000, 0.000000000000000000, 0.000000000000000000 ) ) ;
#18604 = DIRECTION ( 'NONE',  ( 1.000000000000000000, -0.000000000000000000, 6.123233995736764803E-17 ) ) ;
#18605 = CARTESIAN_POINT ( 'NONE',  ( -23.75488095381848197, 42.46645089659918426, 68.50000000000000000 ) ) ;
#18606 = FACE_OUTER_BOUND ( 'NONE', #6816, .T. ) ;
#18607 = DIRECTION ( 'NONE',  ( 0.000000000000000000, 0.000000000000000000, 1.000000000000000000 ) ) ;
#18608 = EDGE_LOOP ( 'NONE', ( #10115, #20066, #11660, #322, #7657, #18339, #1810, #13774, #20904, #14792, #5073, #21141, #17430, #16704, #7789, #9756, #19011, #21713, #11784, #11077, #5925, #18255, #15336, #15950, #5710, #9500, #16799, #16136, #1358, #8936 ) ) ;
#18609 = ORIENTED_EDGE ( 'NONE', *, *, #12416, .T. ) ;
#18610 = ORIENTED_EDGE ( 'NONE', *, *, #15150, .T. ) ;
#18611 = CARTESIAN_POINT ( 'NONE',  ( 14.83748569039513576, 41.93480993936275070, 13.50000000000000000 ) ) ;
#18612 = DIRECTION ( 'NONE',  ( 0.000000000000000000, -0.000000000000000000, -1.000000000000000000 ) ) ;
#18613 = ORIENTED_EDGE ( 'NONE', *, *, #9449, .T. ) ;
#18614 = CIRCLE ( 'NONE', #8976, 1.000000000000000888 ) ;
#18615 = EDGE_CURVE ( 'NONE', #18983, #1780, #3665, .T. ) ;
#18616 = DIRECTION ( 'NONE',  ( 0.000000000000000000, 0.000000000000000000, 1.000000000000000000 ) ) ;
#18617 = VERTEX_POINT ( 'NONE', #20560 ) ;
#18618 = ORIENTED_EDGE ( 'NONE', *, *, #17963, .T. ) ;
#18619 = FACE_OUTER_BOUND ( 'NONE', #2866, .T. ) ;
#18620 = CARTESIAN_POINT ( 'NONE',  ( -31.44597781366221412, 27.99124249474150972, 68.75000000000000000 ) ) ;
#18621 = EDGE_CURVE ( 'NONE', #5475, #6525, #18544, .T. ) ;
#18622 = CIRCLE ( 'NONE', #12940, 1.299999999999999156 ) ;
#18623 = DIRECTION ( 'NONE',  ( 0.000000000000000000, 1.000000000000000000, 0.000000000000000000 ) ) ;
#18624 = ORIENTED_EDGE ( 'NONE', *, *, #10406, .T. ) ;
#18625 = DIRECTION ( 'NONE',  ( 0.000000000000000000, 0.000000000000000000, -1.000000000000000000 ) ) ;
#18626 = DIRECTION ( 'NONE',  ( 1.224646799147353207E-16, 0.000000000000000000, 1.000000000000000000 ) ) ;
#18627 = CIRCLE ( 'NONE', #7211, 0.2999999999999999334 ) ;
#18628 = CARTESIAN_POINT ( 'NONE',  ( -11.70301280599631433, -2.777792850139018999, 68.25000000000000000 ) ) ;
#18629 = ORIENTED_EDGE ( 'NONE', *, *, #1223, .T. ) ;
#18630 = CARTESIAN_POINT ( 'NONE',  ( 9.141460742840918030, -33.93424481021354921, 68.00000000000000000 ) ) ;
#18631 = ORIENTED_EDGE ( 'NONE', *, *, #11467, .T. ) ;
#18632 = DIRECTION ( 'NONE',  ( 0.000000000000000000, -1.000000000000000000, 0.000000000000000000 ) ) ;
#18633 = CIRCLE ( 'NONE', #16110, 0.2999999999999999334 ) ;
#18634 = DIRECTION ( 'NONE',  ( 0.000000000000000000, 0.000000000000000000, 1.000000000000000000 ) ) ;
#18635 = EDGE_LOOP ( 'NONE', ( #19852, #21124, #18161, #8109 ) ) ;
#18636 = ORIENTED_EDGE ( 'NONE', *, *, #7608, .T. ) ;
#18637 = VERTEX_POINT ( 'NONE', #3222 ) ;
#18638 = CARTESIAN_POINT ( 'NONE',  ( -7.347880794884131322E-17, -84.70000000000001705, 1.200000000000002176 ) ) ;
#18639 = EDGE_CURVE ( 'NONE', #19749, #17444, #4930, .T. ) ;
#18640 = AXIS2_PLACEMENT_3D ( 'NONE', #21647, #6100, #18036 ) ;
#18641 = LINE ( 'NONE', #13376, #10724 ) ;
#18642 = TOROIDAL_SURFACE ( 'NONE', #1482, 1.500000000000000000, 0.5000000000000000000 ) ;
#18643 = ORIENTED_EDGE ( 'NONE', *, *, #6976, .T. ) ;
#18644 = FACE_OUTER_BOUND ( 'NONE', #9222, .T. ) ;
#18645 = ORIENTED_EDGE ( 'NONE', *, *, #805, .F. ) ;
#18646 = ORIENTED_EDGE ( 'NONE', *, *, #11561, .F. ) ;
#18647 = DIRECTION ( 'NONE',  ( -0.000000000000000000, -0.000000000000000000, -1.000000000000000000 ) ) ;
#18648 = CARTESIAN_POINT ( 'NONE',  ( -29.37540678000427619, -5.000000000000000000, 3.799999999999999822 ) ) ;
#18649 = EDGE_CURVE ( 'NONE', #22089, #15871, #10268, .T. ) ;
#18650 = EDGE_CURVE ( 'NONE', #1513, #16076, #13384, .T. ) ;
#18651 = ORIENTED_EDGE ( 'NONE', *, *, #21671, .F. ) ;
#18652 = DIRECTION ( 'NONE',  ( -1.000000000000000000, 0.000000000000000000, 0.000000000000000000 ) ) ;
#18653 = ADVANCED_FACE ( 'NONE', ( #1528 ), #5126, .T. ) ;
#18654 = CARTESIAN_POINT ( 'NONE',  ( -30.19999999999999574, 70.00000000000000000, 0.2999999999999996558 ) ) ;
#18655 = FACE_OUTER_BOUND ( 'NONE', #15710, .T. ) ;
#18656 = CARTESIAN_POINT ( 'NONE',  ( -15.95292532278785913, 52.11873716947361856, 14.00000000000000000 ) ) ;
#18657 = ORIENTED_EDGE ( 'NONE', *, *, #21179, .T. ) ;
#18658 = CARTESIAN_POINT ( 'NONE',  ( 23.02398829872513986, 2.502127083158334653, 13.57904421648001225 ) ) ;
#18659 = DIRECTION ( 'NONE',  ( 1.301042606982568087E-14, 0.000000000000000000, 1.000000000000000000 ) ) ;
#18660 = VECTOR ( 'NONE', #15208, 1000.000000000000000 ) ;
#18661 = AXIS2_PLACEMENT_3D ( 'NONE', #9827, #6262, #19907 ) ;
#18662 = DIRECTION ( 'NONE',  ( 0.2309407893632113573, -0.9729678061520313781, -0.000000000000000000 ) ) ;
#18663 = DIRECTION ( 'NONE',  ( -0.000000000000000000, -0.000000000000000000, -1.000000000000000000 ) ) ;
#18664 = VERTEX_POINT ( 'NONE', #13616 ) ;
#18665 = LINE ( 'NONE', #3448, #19132 ) ;
#18666 = ORIENTED_EDGE ( 'NONE', *, *, #14950, .T. ) ;
#18667 = CYLINDRICAL_SURFACE ( 'NONE', #18521, 0.2999999999999999334 ) ;
#18668 = EDGE_CURVE ( 'NONE', #5841, #20665, #1354, .T. ) ;
#18669 = CARTESIAN_POINT ( 'NONE',  ( 1.724728116533979838, 42.31054587065082728, 49.66679706732590915 ) ) ;
#18670 = ORIENTED_EDGE ( 'NONE', *, *, #6744, .F. ) ;
#18671 = ORIENTED_EDGE ( 'NONE', *, *, #15400, .F. ) ;
#18672 = CARTESIAN_POINT ( 'NONE',  ( -8.641460742840918030, 33.93424481021354921, 68.00000000000000000 ) ) ;
#18673 = AXIS2_PLACEMENT_3D ( 'NONE', #4250, #19687, #11064 ) ;
#18674 = CIRCLE ( 'NONE', #1112, 0.6000000000000033085 ) ;
#18675 = ORIENTED_EDGE ( 'NONE', *, *, #19001, .T. ) ;
#18676 = EDGE_CURVE ( 'NONE', #20280, #8695, #14210, .T. ) ;
#18677 = LINE ( 'NONE', #5041, #4929 ) ;
#18678 = EDGE_LOOP ( 'NONE', ( #7663, #3267, #115, #185 ) ) ;
#18679 = DIRECTION ( 'NONE',  ( -0.000000000000000000, -0.000000000000000000, -1.000000000000000000 ) ) ;
#18680 = EDGE_CURVE ( 'NONE', #12963, #1148, #2076, .T. ) ;
#18681 = DIRECTION ( 'NONE',  ( 0.000000000000000000, 0.000000000000000000, -1.000000000000000000 ) ) ;
#18682 = AXIS2_PLACEMENT_3D ( 'NONE', #13997, #19153, #3837 ) ;
#18683 = EDGE_CURVE ( 'NONE', #11429, #9400, #17445, .T. ) ;
#18684 = FACE_OUTER_BOUND ( 'NONE', #5147, .T. ) ;
#18685 = LINE ( 'NONE', #6281, #19172 ) ;
#18686 = CARTESIAN_POINT ( 'NONE',  ( 1.724728116533979616, 43.31054587065082728, 45.76679706732590347 ) ) ;
#18687 = CARTESIAN_POINT ( 'NONE',  ( -31.50000000000002132, -72.00000000000001421, 3.500000000000000000 ) ) ;
#18688 = DIRECTION ( 'NONE',  ( -0.1868663427273192512, 0.9823853469773029534, 0.000000000000000000 ) ) ;
#18689 = CARTESIAN_POINT ( 'NONE',  ( -14.98285978764165449, -51.83353206222920306, 13.49999999999971756 ) ) ;
#18690 = DIRECTION ( 'NONE',  ( -1.000000000000000000, -0.000000000000000000, -0.000000000000000000 ) ) ;
#18691 = VERTEX_POINT ( 'NONE', #6928 ) ;
#18692 = EDGE_CURVE ( 'NONE', #22161, #12166, #1709, .T. ) ;
#18693 = DIRECTION ( 'NONE',  ( -0.2309407893632090258, 0.9729678061520319332, 0.000000000000000000 ) ) ;
#18694 = EDGE_LOOP ( 'NONE', ( #20483, #14137, #14650, #7538 ) ) ;
#18695 = DIRECTION ( 'NONE',  ( 0.000000000000000000, 0.000000000000000000, 1.000000000000000000 ) ) ;
#18696 = ORIENTED_EDGE ( 'NONE', *, *, #3064, .F. ) ;
#18697 = ORIENTED_EDGE ( 'NONE', *, *, #5587, .F. ) ;
#18698 = DIRECTION ( 'NONE',  ( 0.000000000000000000, 0.000000000000000000, -1.000000000000000000 ) ) ;
#18699 = DIRECTION ( 'NONE',  ( -1.000000000000000000, 0.000000000000000000, 0.000000000000000000 ) ) ;
#18700 = EDGE_CURVE ( 'NONE', #6512, #14892, #4230, .T. ) ;
#18701 = ORIENTED_EDGE ( 'NONE', *, *, #360, .T. ) ;
#18702 = ORIENTED_EDGE ( 'NONE', *, *, #7042, .F. ) ;
#18703 = ORIENTED_EDGE ( 'NONE', *, *, #8624, .T. ) ;
#18704 = PRODUCT_DEFINITION_CONTEXT ( 'detailed design', #9155, 'design' ) ;
#18705 = VERTEX_POINT ( 'NONE', #3998 ) ;
#18706 = ADVANCED_FACE ( 'NONE', ( #15724 ), #17624, .T. ) ;
#18707 = DIRECTION ( 'NONE',  ( 0.000000000000000000, 0.000000000000000000, 1.000000000000000000 ) ) ;
#18708 = DIRECTION ( 'NONE',  ( 0.4461977533474357216, 1.626706009486458344E-15, -0.8949343913984425525 ) ) ;
#18709 = CARTESIAN_POINT ( 'NONE',  ( 15.21174975910705918, -51.61873716947361856, 14.00000000000000000 ) ) ;
#18710 = ORIENTED_EDGE ( 'NONE', *, *, #19863, .F. ) ;
#18711 = DIRECTION ( 'NONE',  ( 0.000000000000000000, 0.000000000000000000, 1.000000000000000000 ) ) ;
#18712 = LINE ( 'NONE', #21973, #21561 ) ;
#18713 = CARTESIAN_POINT ( 'NONE',  ( -31.69597781366222122, 56.94165929845684815, 70.50000000000000000 ) ) ;
#18714 = CARTESIAN_POINT ( 'NONE',  ( 25.37540678000427263, 63.74634676501045050, 13.50000000000000000 ) ) ;
#18715 = CARTESIAN_POINT ( 'NONE',  ( -29.50000000000002132, -69.00000000000000000, 0.2999999999999947153 ) ) ;
#18716 = EDGE_LOOP ( 'NONE', ( #19393, #4973, #4002, #1812 ) ) ;
#18717 = DIRECTION ( 'NONE',  ( 0.000000000000000000, 0.000000000000000000, 1.000000000000000000 ) ) ;
#18718 = ORIENTED_EDGE ( 'NONE', *, *, #12297, .F. ) ;
#18719 = ORIENTED_EDGE ( 'NONE', *, *, #17234, .T. ) ;
#18720 = ORIENTED_EDGE ( 'NONE', *, *, #3989, .T. ) ;
#18721 = CARTESIAN_POINT ( 'NONE',  ( -15.95292532278785913, 50.11873716947361856, 13.99999999999999822 ) ) ;
#18722 =( LENGTH_UNIT ( ) NAMED_UNIT ( * ) SI_UNIT ( .MILLI., .METRE. ) );
#18724 = EDGE_CURVE ( 'NONE', #14227, #17330, #7100, .T. ) ;
#18723 = CARTESIAN_POINT ( 'NONE',  ( 1.724728116533979616, 42.36054587065083155, 51.75876104995654003 ) ) ;
#18725 = AXIS2_PLACEMENT_3D ( 'NONE', #9585, #13147, #1068 ) ;
#18726 = EDGE_LOOP ( 'NONE', ( #11101, #20297, #4949, #8056, #20369, #12283, #4328, #18300, #1687, #16566, #4777, #20209, #8255, #16238, #7765, #11368, #17886, #15745, #383, #16947, #13344 ) ) ;
#18727 = ADVANCED_FACE ( 'NONE', ( #7576 ), #19590, .T. ) ;
#18728 = EDGE_CURVE ( 'NONE', #13909, #5745, #539, .T. ) ;
#18729 = CARTESIAN_POINT ( 'NONE',  ( 14.98852729675274986, -51.95836184682382708, 13.85634242029625973 ) ) ;
#18730 = AXIS2_PLACEMENT_3D ( 'NONE', #2905, #7508, #14306 ) ;
#18731 = VERTEX_POINT ( 'NONE', #4203 ) ;
#18732 = PRODUCT_DEFINITION_FORMATION_WITH_SPECIFIED_SOURCE ( 'ANY', '', #11428, .NOT_KNOWN. ) ;
#18733 = DIRECTION ( 'NONE',  ( 1.000000000000000000, 0.000000000000000000, 0.000000000000000000 ) ) ;
#18734 = LINE ( 'NONE', #5327, #987 ) ;
#18735 = LINE ( 'NONE', #1730, #9873 ) ;
#18736 = ORIENTED_EDGE ( 'NONE', *, *, #21806, .T. ) ;
#18737 = CARTESIAN_POINT ( 'NONE',  ( -8.378839169841052481, 41.92645089659918511, 68.06527860057354928 ) ) ;
#18738 = DIRECTION ( 'NONE',  ( 0.000000000000000000, -0.000000000000000000, -1.000000000000000000 ) ) ;
#18739 = FACE_OUTER_BOUND ( 'NONE', #21165, .T. ) ;
#18740 = FILL_AREA_STYLE ('',( #263 ) ) ;
#18741 = ORIENTED_EDGE ( 'NONE', *, *, #12768, .F. ) ;
#18742 = PRODUCT_RELATED_PRODUCT_CATEGORY ( 'part', '', ( #9655 ) ) ;
#18743 = DIRECTION ( 'NONE',  ( -0.000000000000000000, -0.000000000000000000, -1.000000000000000000 ) ) ;
#18744 = FACE_OUTER_BOUND ( 'NONE', #11553, .T. ) ;
#18745 = ORIENTED_EDGE ( 'NONE', *, *, #5875, .F. ) ;
#18746 = DIRECTION ( 'NONE',  ( 0.000000000000000000, -1.000000000000000000, 0.000000000000000000 ) ) ;
#18747 = PLANE ( 'NONE',  #8068 ) ;
#18748 = CARTESIAN_POINT ( 'NONE',  ( -1.724728116533986721, 43.31054587065082728, 27.80876104995653719 ) ) ;
#18749 = VERTEX_POINT ( 'NONE', #9348 ) ;
#18750 = ORIENTED_EDGE ( 'NONE', *, *, #15483, .F. ) ;
#18751 = CIRCLE ( 'NONE', #20551, 0.2999999999999947153 ) ;
#18752 = ORIENTED_EDGE ( 'NONE', *, *, #8552, .F. ) ;
#18753 = DIRECTION ( 'NONE',  ( -0.000000000000000000, 0.000000000000000000, 1.000000000000000000 ) ) ;
#18754 = EDGE_CURVE ( 'NONE', #2833, #9554, #498, .T. ) ;
#18755 = CARTESIAN_POINT ( 'NONE',  ( -4.127054932750482408, 32.93424481021354921, 68.00000000000000000 ) ) ;
#18756 = ADVANCED_FACE ( 'NONE', ( #7350 ), #21000, .T. ) ;
#18757 = ORIENTED_EDGE ( 'NONE', *, *, #20507, .T. ) ;
#18758 = CARTESIAN_POINT ( 'NONE',  ( 1.774728116533979660, 43.26054587065083012, 39.80876104995653719 ) ) ;
#18759 = ORIENTED_EDGE ( 'NONE', *, *, #8000, .T. ) ;
#18760 = LINE ( 'NONE', #3220, #15049 ) ;
#18761 = EDGE_LOOP ( 'NONE', ( #10694, #5232, #408 ) ) ;
#18762 = CARTESIAN_POINT ( 'NONE',  ( -29.13662752439705272, 0.000000000000000000, 7.500000000000000000 ) ) ;
#18763 = CARTESIAN_POINT ( 'NONE',  ( 1.724728116533979616, 43.31054587065082728, 39.70876104995653577 ) ) ;
#18764 = VECTOR ( 'NONE', #16061, 1000.000000000000000 ) ;
#18765 = CARTESIAN_POINT ( 'NONE',  ( 34.39999999999998437, 84.70000000000001705, 79.39999999999999147 ) ) ;
#18766 = AXIS2_PLACEMENT_3D ( 'NONE', #5705, #508, #19221 ) ;
#18767 = DIRECTION ( 'NONE',  ( -0.000000000000000000, 0.000000000000000000, 1.000000000000000000 ) ) ;
#18768 = ORIENTED_EDGE ( 'NONE', *, *, #6257, .F. ) ;
#18769 = CARTESIAN_POINT ( 'NONE',  ( 23.04884263981453785, 2.295195349811796071, 13.26498523032724819 ) ) ;
#18770 = DIRECTION ( 'NONE',  ( 1.000000000000000000, -0.000000000000000000, 0.000000000000000000 ) ) ;
#18771 = FACE_OUTER_BOUND ( 'NONE', #14786, .T. ) ;
#18772 = PRODUCT_DEFINITION_SHAPE ( 'NONE', 'NONE',  #2891 ) ;
#18773 = DIRECTION ( 'NONE',  ( -1.445602896647331422E-15, 0.000000000000000000, -1.000000000000000000 ) ) ;
#18774 = ORIENTED_EDGE ( 'NONE', *, *, #9592, .T. ) ;
#18775 = DIRECTION ( 'NONE',  ( 0.000000000000000000, 0.000000000000000000, 1.000000000000000000 ) ) ;
#18776 = CARTESIAN_POINT ( 'NONE',  ( -0.000000000000000000, 26.24124249474150972, 68.50000000000000000 ) ) ;
#18777 = ORIENTED_EDGE ( 'NONE', *, *, #20467, .T. ) ;
#18778 = CIRCLE ( 'NONE', #9122, 0.5000000000000000000 ) ;
#18779 = CARTESIAN_POINT ( 'NONE',  ( 31.50000000000002132, -71.70000000000001705, 3.500000000000000000 ) ) ;
#18780 = ADVANCED_FACE ( 'NONE', ( #21224 ), #22099, .T. ) ;
#18781 = DIRECTION ( 'NONE',  ( -1.000000000000000000, -0.000000000000000000, 0.000000000000000000 ) ) ;
#18782 = CIRCLE ( 'NONE', #10551, 0.5000000000000004441 ) ;
#18783 = EDGE_LOOP ( 'NONE', ( #5366, #19961, #5903, #8359 ) ) ;
#18784 = AXIS2_PLACEMENT_3D ( 'NONE', #20438, #18743, #13260 ) ;
#18785 = CIRCLE ( 'NONE', #8070, 2.000000000000000000 ) ;
#18786 = DIRECTION ( 'NONE',  ( 0.000000000000000000, 0.000000000000000000, 1.000000000000000000 ) ) ;
#18787 = ORIENTED_EDGE ( 'NONE', *, *, #18440, .T. ) ;
#18788 = LINE ( 'NONE', #18451, #13842 ) ;
#18789 = VERTEX_POINT ( 'NONE', #12351 ) ;
#18790 = LINE ( 'NONE', #3466, #970 ) ;
#18791 = CARTESIAN_POINT ( 'NONE',  ( 28.87540678000427619, 6.494748934539263274, 13.50000000000000000 ) ) ;
#18792 = AXIS2_PLACEMENT_3D ( 'NONE', #8316, #16256, #1579 ) ;
#18793 = DIRECTION ( 'NONE',  ( 0.000000000000000000, -0.000000000000000000, -1.000000000000000000 ) ) ;
#18794 = CARTESIAN_POINT ( 'NONE',  ( 1.724728116533979838, 43.31054587065082728, 41.66679706732590915 ) ) ;
#18795 = ADVANCED_FACE ( 'NONE', ( #17524 ), #5690, .T. ) ;
#18796 = LINE ( 'NONE', #18686, #4278 ) ;
#18797 = AXIS2_PLACEMENT_3D ( 'NONE', #10970, #12293, #19047 ) ;
#18798 = CIRCLE ( 'NONE', #21665, 2.076718556943725424 ) ;
#18799 = TOROIDAL_SURFACE ( 'NONE', #13419, 0.05000000000000000278, 0.05000000000000000278 ) ;
#18800 = DIRECTION ( 'NONE',  ( 0.000000000000000000, 0.000000000000000000, -1.000000000000000000 ) ) ;
#18801 = CARTESIAN_POINT ( 'NONE',  ( 25.37540678000427263, 63.74634676501045050, 3.799999999999999822 ) ) ;
#18802 = ORIENTED_EDGE ( 'NONE', *, *, #8438, .F. ) ;
#18803 = EDGE_CURVE ( 'NONE', #5223, #9561, #614, .T. ) ;
#18804 = FACE_OUTER_BOUND ( 'NONE', #11116, .T. ) ;
#18805 = CARTESIAN_POINT ( 'NONE',  ( 9.141460742840918030, -32.61873716947361856, 68.00000000000000000 ) ) ;
#18806 = EDGE_CURVE ( 'NONE', #8904, #19806, #13500, .T. ) ;
#18807 = DIRECTION ( 'NONE',  ( 0.000000000000000000, 0.000000000000000000, 1.000000000000000000 ) ) ;
#18808 = CIRCLE ( 'NONE', #12001, 0.2500000000000002220 ) ;
#18809 = AXIS2_PLACEMENT_3D ( 'NONE', #15253, #16709, #15139 ) ;
#18810 = ORIENTED_EDGE ( 'NONE', *, *, #6362, .F. ) ;
#18811 = AXIS2_PLACEMENT_3D ( 'NONE', #6594, #18213, #16750 ) ;
#18812 = VERTEX_POINT ( 'NONE', #3763 ) ;
#18813 = CARTESIAN_POINT ( 'NONE',  ( -14.71174975910705029, 51.61873716947361856, 68.00000000000000000 ) ) ;
#18814 = EDGE_CURVE ( 'NONE', #15951, #18912, #11026, .T. ) ;
#18815 = CARTESIAN_POINT ( 'NONE',  ( 0.000000000000000000, 0.000000000000000000, 0.000000000000000000 ) ) ;
#18816 = ORIENTED_EDGE ( 'NONE', *, *, #20709, .T. ) ;
#18817 = CIRCLE ( 'NONE', #14497, 0.6999999999999992895 ) ;
#18818 = ORIENTED_EDGE ( 'NONE', *, *, #14962, .T. ) ;
#18819 = EDGE_LOOP ( 'NONE', ( #15037, #2631, #3441, #9664 ) ) ;
#18820 = DIRECTION ( 'NONE',  ( -0.000000000000000000, 1.000000000000000000, -0.000000000000000000 ) ) ;
#18821 = EDGE_CURVE ( 'NONE', #7404, #3943, #2521, .T. ) ;
#18822 = DIRECTION ( 'NONE',  ( 0.000000000000000000, 0.000000000000000000, -1.000000000000000000 ) ) ;
#18823 = VECTOR ( 'NONE', #20588, 1000.000000000000000 ) ;
#18824 = AXIS2_PLACEMENT_3D ( 'NONE', #8449, #20537, #259 ) ;
#18825 = VECTOR ( 'NONE', #18527, 1000.000000000000000 ) ;
#18826 = LINE ( 'NONE', #10335, #285 ) ;
#18827 = VECTOR ( 'NONE', #8687, 1000.000000000000000 ) ;
#18828 = DIRECTION ( 'NONE',  ( -0.000000000000000000, 1.000000000000000000, 0.000000000000000000 ) ) ;
#18829 = CARTESIAN_POINT ( 'NONE',  ( -23.02398829872514341, 3.052854503364687666, 13.54964687161600700 ) ) ;
#18830 = FACE_OUTER_BOUND ( 'NONE', #14009, .T. ) ;
#18831 = DIRECTION ( 'NONE',  ( 0.000000000000000000, 0.000000000000000000, -1.000000000000000000 ) ) ;
#18832 = CARTESIAN_POINT ( 'NONE',  ( 15.21174975910705918, -52.39333383871510108, 13.50000000000000000 ) ) ;
#18833 = AXIS2_PLACEMENT_3D ( 'NONE', #11304, #4161, #19718 ) ;
#18834 = DIRECTION ( 'NONE',  ( 0.000000000000000000, 1.000000000000000000, 0.000000000000000000 ) ) ;
#18835 = EDGE_CURVE ( 'NONE', #22033, #5083, #19230, .T. ) ;
#18836 = EDGE_LOOP ( 'NONE', ( #5912, #12487, #12269, #17096 ) ) ;
#18837 = ORIENTED_EDGE ( 'NONE', *, *, #4576, .F. ) ;
#18838 = LINE ( 'NONE', #1593, #5305 ) ;
#18839 = EDGE_CURVE ( 'NONE', #10704, #13437, #17403, .T. ) ;
#18840 = LINE ( 'NONE', #7314, #21719 ) ;
#18841 = ORIENTED_EDGE ( 'NONE', *, *, #6240, .T. ) ;
#18842 = AXIS2_PLACEMENT_3D ( 'NONE', #10459, #21200, #8773 ) ;
#18843 = CLOSED_SHELL ( 'NONE', ( #3888, #20055, #19103, #9375, #9976, #9503, #18118, #12638, #10772, #6641, #16267, #7450, #10732, #20432, #129, #9238, #17210, #5436, #13737, #7369, #10965, #8927, #3802, #19823, #719, #15736, #14626, #14262, #7483, #9510, #11556, #21244, #2435, #4393, #7433, #8013, #17673, #18004, #10011, #21553, #20858, #12496, #11453, #11609, #12442, #21860, #11972, #3094, #20034, #19506, #12597, #3142, #13385, #9633, #21520, #7224, #6634, #17838, #19180, #14037, #2544, #18321, #3522, #1365, #22024, #20335, #10306, #21118, #6008, #10227, #5490, #9050, #15020, #15113, #19064, #7979, #19248, #12182, #10357, #8312, #13467, #6573, #9119, #2477, #19892, #3358, #95, #11535, #10193, #15104, #4377, #7566, #7098, #8189, #16444, #14721, #19482, #17028, #1280, #19017, #5779, #667, #1539, #6836, #1819, #9596, #13572, #15136, #20743, #5127, #17631, #16761, #3283, #1387, #15785, #12792, #8883, #2818, #22095, #14143, #15980, #6191, #13196, #18706, #20162, #9268, #10642, #1313, #7411, #19985, #1250, #15036, #1157, #17834, #16853, #2176, #5398, #4714, #18164, #1919, #18727, #9840, #17485, #7142, #18391, #300, #6709, #11288, #5094, #7549, #21421, #19341, #14810, #16743, #12494, #8580, #6857, #20333, #3417, #5853, #11391, #14301, #10520, #335, #12742, #18491, #16755, #14850, #12035, #19478, #15772, #790, #13207, #9067, #16229, #13484, #18653, #19983, #1873, #4427, #8989, #7486, #14156, #18226, #3475, #4179, #4913, #1716, #17961, #1608, #16565, #11666, #13884, #4803, #12101, #15321, #20616, #17131, #19774, #12329, #7079, #2821, #5535, #12569, #6648, #9355, #20835, #15064, #13735, #15997, #21261, #9081, #1187, #15634, #12304, #4469, #1667, #3761, #7575, #5196, #13627, #9693, #19770, #890, #14237, #5046, #2105, #16587, #16922, #5071, #18780, #8059, #6170, #10079, #17590, #188, #2938, #16085, #7802, #16823, #2228, #13833, #2482, #13471, #22109, #11052, #7392, #15497, #16585, #20102, #19500, #11226, #19771, #11421, #15531, #3987, #11142, #5983, #13314, #21830, #1088, #15039, #17634, #4859, #18526, #8700, #13989, #2903, #3015, #12490, #9705, #10676, #11595, #10955, #13962, #17262, #3854, #3886, #19343, #14796, #8885, #7503, #19354, #80, #6115, #13562, #18579, #16782, #18367, #7890, #8376, #19436, #7932, #1893, #9116, #10864, #5193, #17985, #15807, #19263, #17931, #2827, #2265, #17030, #22114, #8284, #9092, #17999, #14995, #16027, #15353, #5054, #4234, #5229, #21161, #8806, #10743, #9492, #21531, #17346, #18532, #18013, #1966, #4029, #6291, #6725, #17696, #17090, #3450, #18875, #14777, #2790, #15650, #2073, #15676, #6171, #13281, #12524, #12366, #7076, #10380, #3735, #6640, #6616, #12141, #21457, #8074, #18385, #15666, #9621, #14562, #19752, #11681, #5248, #11261, #5149, #16520, #5087, #18083, #13049, #9403, #4037, #17000, #17836, #11497, #5333, #2226, #19371, #8272, #7510 ) ) ;
#18844 = VECTOR ( 'NONE', #13959, 1000.000000000000000 ) ;
#18845 = VECTOR ( 'NONE', #9860, 1000.000000000000000 ) ;
#18846 = CARTESIAN_POINT ( 'NONE',  ( 17.95292532278785913, 38.74634676501045760, 42.50000000000000000 ) ) ;
#18847 = AXIS2_PLACEMENT_3D ( 'NONE', #19515, #7999, #14803 ) ;
#18848 = CARTESIAN_POINT ( 'NONE',  ( -1.724728116533986721, 43.31054587065082728, 47.80876104995653719 ) ) ;
#18849 = AXIS2_PLACEMENT_3D ( 'NONE', #3653, #8588, #18872 ) ;
#18850 = CARTESIAN_POINT ( 'NONE',  ( -1.824728116533986810, 42.36054587065083155, 35.70876104995653577 ) ) ;
#18851 = FACE_OUTER_BOUND ( 'NONE', #4792, .T. ) ;
#18852 = DIRECTION ( 'NONE',  ( -1.000000000000000000, 0.000000000000000000, 0.000000000000000000 ) ) ;
#18853 = ORIENTED_EDGE ( 'NONE', *, *, #3580, .F. ) ;
#18854 = DIRECTION ( 'NONE',  ( -1.000000000000000000, 0.000000000000000000, 0.000000000000000000 ) ) ;
#18855 = FACE_OUTER_BOUND ( 'NONE', #19827, .T. ) ;
#18856 = EDGE_CURVE ( 'NONE', #2670, #21314, #14268, .T. ) ;
#18857 = EDGE_CURVE ( 'NONE', #2743, #19660, #6122, .T. ) ;
#18858 = CARTESIAN_POINT ( 'NONE',  ( 1.724728116533979616, 43.26054587065083012, 43.75876104995653293 ) ) ;
#18859 = DIRECTION ( 'NONE',  ( 0.000000000000000000, 0.000000000000000000, -1.000000000000000000 ) ) ;
#18860 = VECTOR ( 'NONE', #21835, 1000.000000000000000 ) ;
#18861 = CIRCLE ( 'NONE', #20279, 0.04999999999999991257 ) ;
#18862 = DIRECTION ( 'NONE',  ( 1.734723475976806848E-16, 0.000000000000000000, -1.000000000000000000 ) ) ;
#18863 = ORIENTED_EDGE ( 'NONE', *, *, #3505, .F. ) ;
#18864 = DIRECTION ( 'NONE',  ( 1.000000000000000000, 0.000000000000000000, 0.000000000000000000 ) ) ;
#18865 = CYLINDRICAL_SURFACE ( 'NONE', #2335, 0.2999999999999999334 ) ;
#18866 = AXIS2_PLACEMENT_3D ( 'NONE', #718, #2403, #12138 ) ;
#18867 = DIRECTION ( 'NONE',  ( 0.000000000000000000, 0.000000000000000000, 1.000000000000000000 ) ) ;
#18868 = EDGE_LOOP ( 'NONE', ( #14932, #19979, #906 ) ) ;
#18869 = EDGE_LOOP ( 'NONE', ( #9766, #71, #12346, #19329 ) ) ;
#18870 = VECTOR ( 'NONE', #21108, 1000.000000000000000 ) ;
#18871 = ORIENTED_EDGE ( 'NONE', *, *, #6779, .T. ) ;
#18872 = DIRECTION ( 'NONE',  ( 1.000000000000000000, 0.000000000000000000, 0.000000000000000000 ) ) ;
#18873 = LINE ( 'NONE', #3548, #15282 ) ;
#18874 = AXIS2_PLACEMENT_3D ( 'NONE', #18358, #7871, #11305 ) ;
#18875 = ADVANCED_FACE ( 'NONE', ( #9573 ), #10307, .T. ) ;
#18876 = DIRECTION ( 'NONE',  ( 1.000000000000000000, 0.000000000000000000, 0.000000000000000000 ) ) ;
#18877 = FACE_OUTER_BOUND ( 'NONE', #3908, .T. ) ;
#18878 = EDGE_LOOP ( 'NONE', ( #14437, #4467, #10526, #11978 ) ) ;
#18879 = DIRECTION ( 'NONE',  ( -1.095978537872987122E-16, -0.4461977533474360547, -0.8949343913984424415 ) ) ;
#18880 = VECTOR ( 'NONE', #2739, 1000.000000000000000 ) ;
#18881 = TOROIDAL_SURFACE ( 'NONE', #5666, 1.750000000000000000, 0.2500000000000000000 ) ;
#18882 = EDGE_LOOP ( 'NONE', ( #3182, #9533, #17402, #16818, #7996, #8694, #3465, #3115 ) ) ;
#18883 = CARTESIAN_POINT ( 'NONE',  ( -23.26572410265623958, -3.298136152264965038, 13.49420500573782888 ) ) ;
#18884 = CARTESIAN_POINT ( 'NONE',  ( -15.21174975910705207, -52.39333383871510108, 13.79999999999999893 ) ) ;
#18885 = TOROIDAL_SURFACE ( 'NONE', #19960, 4.700000000000000178, 0.2999999999999999889 ) ;
#18886 = LINE ( 'NONE', #3562, #20810 ) ;
#18887 = VECTOR ( 'NONE', #18698, 1000.000000000000000 ) ;
#18888 = DIRECTION ( 'NONE',  ( 0.000000000000000000, 0.000000000000000000, 1.000000000000000000 ) ) ;
#18889 = VERTEX_POINT ( 'NONE', #11351 ) ;
#18890 = CARTESIAN_POINT ( 'NONE',  ( 23.07496371939382129, 2.433385307706760869, 13.33569868627438382 ) ) ;
#18891 = AXIS2_PLACEMENT_3D ( 'NONE', #19874, #4539, #18190 ) ;
#18892 = CARTESIAN_POINT ( 'NONE',  ( -1.724728116533986721, 42.36054587065083155, 53.76679706732590347 ) ) ;
#18893 = EDGE_CURVE ( 'NONE', #20293, #9425, #19955, .T. ) ;
#18894 = CARTESIAN_POINT ( 'NONE',  ( 0.000000000000000000, 26.24124249474150972, 70.25000000000000000 ) ) ;
#18895 = CARTESIAN_POINT ( 'NONE',  ( -4.127054932750482408, -33.93424481021354921, 68.50000000000000000 ) ) ;
#18896 = ORIENTED_EDGE ( 'NONE', *, *, #226, .T. ) ;
#18897 = ADVANCED_FACE ( 'NONE', ( #4317 ), #11129, .T. ) ;
#18898 = CARTESIAN_POINT ( 'NONE',  ( -21.71259690522456154, 45.22582864897715638, 68.50000000000000000 ) ) ;
#18899 = FACE_OUTER_BOUND ( 'NONE', #1583, .T. ) ;
#18900 = CONICAL_SURFACE ( 'NONE', #17806, 0.9652499999999990532, 0.06981317007976590994 ) ;
#18901 = ORIENTED_EDGE ( 'NONE', *, *, #1574, .F. ) ;
#18902 = DIRECTION ( 'NONE',  ( -0.000000000000000000, 0.000000000000000000, 1.000000000000000000 ) ) ;
#18903 = CARTESIAN_POINT ( 'NONE',  ( 17.45292532278785913, -50.11873716947361856, 68.50000000000000000 ) ) ;
#18904 = AXIS2_PLACEMENT_3D ( 'NONE', #3771, #17299, #1965 ) ;
#18905 = AXIS2_PLACEMENT_3D ( 'NONE', #2154, #5646, #14007 ) ;
#18906 = VERTEX_POINT ( 'NONE', #19864 ) ;
#18907 = DIRECTION ( 'NONE',  ( -1.000000000000000000, 0.000000000000000000, -0.000000000000000000 ) ) ;
#18908 = AXIS2_PLACEMENT_3D ( 'NONE', #9498, #11278, #2789 ) ;
#18909 = ORIENTED_EDGE ( 'NONE', *, *, #5162, .T. ) ;
#18910 = EDGE_CURVE ( 'NONE', #17808, #10531, #6009, .T. ) ;
#18911 = CARTESIAN_POINT ( 'NONE',  ( -13.37248138918699425, 42.46645089659917716, 69.50000000000000000 ) ) ;
#18912 = VERTEX_POINT ( 'NONE', #2863 ) ;
#18913 = DIRECTION ( 'NONE',  ( 1.000000000000000000, 0.000000000000000000, 0.000000000000000000 ) ) ;
#18914 = AXIS2_PLACEMENT_3D ( 'NONE', #15151, #13593, #3198 ) ;
#18915 = CIRCLE ( 'NONE', #18179, 1.299999999999999156 ) ;
#18916 = CARTESIAN_POINT ( 'NONE',  ( 27.67540678000426269, 36.74634676501047181, 13.50000000000000000 ) ) ;
#18917 = CARTESIAN_POINT ( 'NONE',  ( 14.71174975910705740, 32.10873716947361345, 13.75000000000000000 ) ) ;
#18918 = EDGE_CURVE ( 'NONE', #4113, #6512, #7792, .T. ) ;
#18919 = CARTESIAN_POINT ( 'NONE',  ( 15.95292532278785913, 52.11873716947361856, 109.6002446535588319 ) ) ;
#18920 = EDGE_CURVE ( 'NONE', #1239, #8409, #5653, .T. ) ;
#18921 = TOROIDAL_SURFACE ( 'NONE', #6774, 0.5999999999999999778, 0.2999999999999999889 ) ;
#18922 = CARTESIAN_POINT ( 'NONE',  ( -1.824728116533986810, 42.36054587065083155, 33.76679706732591058 ) ) ;
#18923 = CIRCLE ( 'NONE', #15331, 1.984122918275927239 ) ;
#18924 = DIRECTION ( 'NONE',  ( 0.000000000000000000, 0.000000000000000000, -1.000000000000000000 ) ) ;
#18925 = DIRECTION ( 'NONE',  ( 0.000000000000000000, 0.000000000000000000, -1.000000000000000000 ) ) ;
#18926 = VERTEX_POINT ( 'NONE', #14811 ) ;
#18927 = CARTESIAN_POINT ( 'NONE',  ( -21.67365502786443088, 45.72430987248279166, 68.50000000000000000 ) ) ;
#18928 = CARTESIAN_POINT ( 'NONE',  ( -1.824728116533986810, 43.31054587065082728, 29.66679706732590560 ) ) ;
#18929 = ORIENTED_EDGE ( 'NONE', *, *, #10693, .T. ) ;
#18930 = EDGE_LOOP ( 'NONE', ( #17946, #18315, #3221, #17870 ) ) ;
#18931 = SPHERICAL_SURFACE ( 'NONE', #12788, 0.2500000000000000000 ) ;
#18932 = EDGE_CURVE ( 'NONE', #12734, #3260, #8008, .T. ) ;
#18933 = ORIENTED_EDGE ( 'NONE', *, *, #7308, .F. ) ;
#18934 = AXIS2_PLACEMENT_3D ( 'NONE', #6469, #4221, #19657 ) ;
#18935 = TOROIDAL_SURFACE ( 'NONE', #17840, 2.274596669241483848, 0.2999999999999999889 ) ;
#18936 = DIRECTION ( 'NONE',  ( 0.000000000000000000, -0.000000000000000000, -1.000000000000000000 ) ) ;
#18937 = ORIENTED_EDGE ( 'NONE', *, *, #17544, .F. ) ;
#18938 = ORIENTED_EDGE ( 'NONE', *, *, #18261, .T. ) ;
#18939 = EDGE_CURVE ( 'NONE', #497, #15133, #11232, .T. ) ;
#18940 = DIRECTION ( 'NONE',  ( 0.000000000000000000, 0.000000000000000000, 1.000000000000000000 ) ) ;
#18941 = LINE ( 'NONE', #3714, #7379 ) ;
#18942 = EDGE_CURVE ( 'NONE', #4947, #14127, #11462, .T. ) ;
#18943 = CARTESIAN_POINT ( 'NONE',  ( 23.02398829872514341, 2.623740515231442583, 13.63037280509750993 ) ) ;
#18944 = CARTESIAN_POINT ( 'NONE',  ( -1.724728116533986721, 43.31054587065082728, 45.71679706732590631 ) ) ;
#18945 =( NAMED_UNIT ( * ) SI_UNIT ( $, .STERADIAN. ) SOLID_ANGLE_UNIT ( ) );
#18946 = AXIS2_PLACEMENT_3D ( 'NONE', #1764, #20126, #9940 ) ;
#18947 = CIRCLE ( 'NONE', #1076, 1.984122918275925462 ) ;
#18948 = CIRCLE ( 'NONE', #1057, 0.05000000000000143219 ) ;
#18949 = CARTESIAN_POINT ( 'NONE',  ( -9.141460742840918030, -33.43424481021354921, 7.321391277662001151 ) ) ;
#18950 = CARTESIAN_POINT ( 'NONE',  ( 1.724728116533979616, 43.26054587065083012, 27.80876104995653719 ) ) ;
#18951 = CARTESIAN_POINT ( 'NONE',  ( 26.37540678000427619, -10.94079601157914716, 42.50000000000000000 ) ) ;
#18952 = CARTESIAN_POINT ( 'NONE',  ( -1.724728116533986721, 42.31054587065082728, 37.66679706732590915 ) ) ;
#18953 = ORIENTED_EDGE ( 'NONE', *, *, #9663, .T. ) ;
#18954 = ORIENTED_EDGE ( 'NONE', *, *, #5862, .F. ) ;
#18955 = CARTESIAN_POINT ( 'NONE',  ( 14.96174975910706628, 41.81054587065081307, 13.62426406871193230 ) ) ;
#18956 = DIRECTION ( 'NONE',  ( 0.000000000000000000, 0.000000000000000000, 1.000000000000000000 ) ) ;
#18957 = EDGE_CURVE ( 'NONE', #17693, #13182, #16389, .T. ) ;
#18958 = ORIENTED_EDGE ( 'NONE', *, *, #18668, .T. ) ;
#18959 = DIRECTION ( 'NONE',  ( -0.000000000000000000, 1.000000000000000000, -0.000000000000000000 ) ) ;
#18960 = AXIS2_PLACEMENT_3D ( 'NONE', #16934, #11673, #13683 ) ;
#18961 = AXIS2_PLACEMENT_3D ( 'NONE', #10766, #15999, #17474 ) ;
#18962 = PRODUCT_DEFINITION_SHAPE ( 'NONE', 'NONE',  #22177 ) ;
#18963 = LINE ( 'NONE', #13783, #23 ) ;
#18964 = CARTESIAN_POINT ( 'NONE',  ( -1.724728116533986721, 42.36054587065083155, 27.70876104995653577 ) ) ;
#18965 = EDGE_CURVE ( 'NONE', #10812, #483, #9219, .T. ) ;
#18966 = CARTESIAN_POINT ( 'NONE',  ( 17.95292532278785913, -38.74634676501045760, 109.6002446535588319 ) ) ;
#18967 = ADVANCED_FACE ( 'NONE', ( #9795 ), #21747, .T. ) ;
#18968 = DIRECTION ( 'NONE',  ( 0.000000000000000000, -1.000000000000000000, 0.000000000000000000 ) ) ;
#18969 = ORIENTED_EDGE ( 'NONE', *, *, #5140, .F. ) ;
#18970 = DIRECTION ( 'NONE',  ( 1.000000000000000000, -0.000000000000000000, 0.000000000000000000 ) ) ;
#18971 = EDGE_CURVE ( 'NONE', #8303, #12842, #14929, .T. ) ;
#18972 = DIRECTION ( 'NONE',  ( 0.000000000000000000, 1.000000000000000000, 0.000000000000000000 ) ) ;
#18973 = DIRECTION ( 'NONE',  ( -1.000000000000000000, 0.000000000000000000, 0.000000000000000000 ) ) ;
#18974 = DIRECTION ( 'NONE',  ( 1.000000000000000000, 0.000000000000000000, 0.000000000000000000 ) ) ;
#18975 = DIRECTION ( 'NONE',  ( 1.000000000000000000, 0.000000000000000000, 0.000000000000000000 ) ) ;
#18976 = CARTESIAN_POINT ( 'NONE',  ( -14.96174975910705207, 51.86873716947361856, 68.00000000000000000 ) ) ;
#18977 = TOROIDAL_SURFACE ( 'NONE', #12164, 0.05000000000000000278, 0.05000000000000000278 ) ;
#18978 = DIRECTION ( 'NONE',  ( -1.000000000000000000, -0.000000000000000000, -0.000000000000000000 ) ) ;
#18979 = VECTOR ( 'NONE', #21808, 1000.000000000000000 ) ;
#18980 = CARTESIAN_POINT ( 'NONE',  ( -1.774728116533986766, 43.26054587065083012, 20.00000000000000000 ) ) ;
#18981 = DIRECTION ( 'NONE',  ( 0.000000000000000000, 1.000000000000000000, 0.000000000000000000 ) ) ;
#18982 = ORIENTED_EDGE ( 'NONE', *, *, #9967, .F. ) ;
#18983 = VERTEX_POINT ( 'NONE', #14928 ) ;
#18984 = ORIENTED_EDGE ( 'NONE', *, *, #1967, .F. ) ;
#18985 = CARTESIAN_POINT ( 'NONE',  ( 1.724728116533979616, 43.26054587065083012, 43.80876104995653719 ) ) ;
#18986 = CARTESIAN_POINT ( 'NONE',  ( 1.724728116533979616, 43.31054587065082728, 51.70876104995653577 ) ) ;
#18987 = ADVANCED_FACE ( 'NONE', ( #21781 ), #150, .F. ) ;
#18988 = DIRECTION ( 'NONE',  ( 0.000000000000000000, 0.000000000000000000, 1.000000000000000000 ) ) ;
#18989 = EDGE_CURVE ( 'NONE', #4433, #12433, #15647, .T. ) ;
#18990 = AXIS2_PLACEMENT_3D ( 'NONE', #707, #17505, #7556 ) ;
#18991 = VERTEX_POINT ( 'NONE', #1501 ) ;
#18992 = CARTESIAN_POINT ( 'NONE',  ( 31.63662752439705272, 0.000000000000000000, 1.500000000000001332 ) ) ;
#18993 = EDGE_LOOP ( 'NONE', ( #3042, #11404, #4036, #6314, #4291, #21221, #1949, #12127 ) ) ;
#18994 = DIRECTION ( 'NONE',  ( 0.000000000000000000, 0.000000000000000000, 1.000000000000000000 ) ) ;
#18995 = AXIS2_PLACEMENT_3D ( 'NONE', #19818, #2814, #11745 ) ;
#18996 = CARTESIAN_POINT ( 'NONE',  ( 1.724728116533979616, 43.31054587065082728, 49.76679706732591058 ) ) ;
#18997 = DIRECTION ( 'NONE',  ( 0.000000000000000000, 1.000000000000000000, 0.000000000000000000 ) ) ;
#18998 = DIRECTION ( 'NONE',  ( 1.038507728162729222E-16, 1.000000000000000000, -1.271805165184275985E-32 ) ) ;
#18999 = EDGE_LOOP ( 'NONE', ( #22047, #15831, #14774, #7555 ) ) ;
#19000 = FACE_OUTER_BOUND ( 'NONE', #8358, .T. ) ;
#19001 = EDGE_CURVE ( 'NONE', #2851, #21143, #18734, .T. ) ;
#19002 = CIRCLE ( 'NONE', #402, 1.000000000000000888 ) ;
#19003 = DIRECTION ( 'NONE',  ( 0.000000000000000000, 0.000000000000000000, -1.000000000000000000 ) ) ;
#19004 = CARTESIAN_POINT ( 'NONE',  ( 26.37540678000427619, -10.94079601157914716, 13.50000000000000000 ) ) ;
#19005 = VERTEX_POINT ( 'NONE', #51 ) ;
#19006 = DIRECTION ( 'NONE',  ( -0.000000000000000000, 1.000000000000000000, 0.000000000000000000 ) ) ;
#19007 = AXIS2_PLACEMENT_3D ( 'NONE', #19351, #21154, #5826 ) ;
#19008 = VECTOR ( 'NONE', #15126, 1000.000000000000000 ) ;
#19009 = TOROIDAL_SURFACE ( 'NONE', #2208, 1.300000000000000044, 0.2999999999999999889 ) ;
#19010 = CARTESIAN_POINT ( 'NONE',  ( -35.00000000000001421, 85.00000000000000000, 78.50000000000000000 ) ) ;
#19011 = ORIENTED_EDGE ( 'NONE', *, *, #17545, .T. ) ;
#19012 = DIRECTION ( 'NONE',  ( -0.2309407893632113573, 0.9729678061520313781, 0.000000000000000000 ) ) ;
#19013 = DIRECTION ( 'NONE',  ( -1.000000000000000000, 0.000000000000000000, -0.000000000000000000 ) ) ;
#19014 = EDGE_LOOP ( 'NONE', ( #18229, #19952, #13497, #21862 ) ) ;
#19015 = EDGE_CURVE ( 'NONE', #2324, #8427, #20294, .T. ) ;
#19016 = ORIENTED_EDGE ( 'NONE', *, *, #6782, .T. ) ;
#19017 = ADVANCED_FACE ( 'NONE', ( #20647 ), #6567, .T. ) ;
#19018 = CIRCLE ( 'NONE', #4719, 0.3000000000000016542 ) ;
#19019 = AXIS2_PLACEMENT_3D ( 'NONE', #10869, #1917, #20740 ) ;
#19020 = ORIENTED_EDGE ( 'NONE', *, *, #9134, .T. ) ;
#19021 = VECTOR ( 'NONE', #15667, 1000.000000000000000 ) ;
#19022 = AXIS2_PLACEMENT_3D ( 'NONE', #647, #16080, #860 ) ;
#19023 = TOROIDAL_SURFACE ( 'NONE', #9369, 0.2999999999999999889, 0.2999999999999999889 ) ;
#19024 = CARTESIAN_POINT ( 'NONE',  ( 27.37540678000427619, 5.683640910026986681, 42.50000000000000000 ) ) ;
#19025 = DIRECTION ( 'NONE',  ( 0.000000000000000000, 0.000000000000000000, 1.000000000000000000 ) ) ;
#19026 = CARTESIAN_POINT ( 'NONE',  ( -1.724728116533986721, 42.36054587065083155, 49.71679706732589921 ) ) ;
#19027 = UNCERTAINTY_MEASURE_WITH_UNIT (LENGTH_MEASURE( 1.000000000000000082E-05 ), #3960, 'distance_accuracy_value', 'NONE');
#19028 = DIRECTION ( 'NONE',  ( 1.000000000000000000, -0.000000000000000000, 0.000000000000000000 ) ) ;
#19029 = CARTESIAN_POINT ( 'NONE',  ( 1.724728116533979838, 43.31054587065082728, 29.71679706732590631 ) ) ;
#19030 = CARTESIAN_POINT ( 'NONE',  ( -9.178906393579158163, 42.46645089659918426, 70.38908280829822672 ) ) ;
#19031 = PRODUCT_DEFINITION ( 'UNKNOWN', '', #12625, #20819 ) ;
#19032 = ORIENTED_EDGE ( 'NONE', *, *, #7981, .T. ) ;
#19033 = VECTOR ( 'NONE', #7065, 1000.000000000000000 ) ;
#19034 = DIRECTION ( 'NONE',  ( 0.000000000000000000, 0.000000000000000000, 1.000000000000000000 ) ) ;
#19035 = DIRECTION ( 'NONE',  ( 0.000000000000000000, 0.000000000000000000, 1.000000000000000000 ) ) ;
#19036 = STYLED_ITEM ( 'NONE', ( #17271 ), #13188 ) ;
#19037 = ORIENTED_EDGE ( 'NONE', *, *, #2626, .T. ) ;
#19038 = ORIENTED_EDGE ( 'NONE', *, *, #15726, .F. ) ;
#19039 = DIRECTION ( 'NONE',  ( 0.000000000000000000, 0.000000000000000000, -1.000000000000000000 ) ) ;
#19040 = APPLICATION_PROTOCOL_DEFINITION ( 'draft international standard', 'automotive_design', 1998, #419 ) ;
#19041 = ADVANCED_FACE ( 'NONE', ( #12116 ), #15145, .T. ) ;
#19042 = ORIENTED_EDGE ( 'NONE', *, *, #17246, .F. ) ;
#19043 = AXIS2_PLACEMENT_3D ( 'NONE', #11327, #20077, #9549 ) ;
#19044 = CARTESIAN_POINT ( 'NONE',  ( 23.02398829872513986, -3.264233419183535378, 13.78834712654929717 ) ) ;
#19045 = ORIENTED_EDGE ( 'NONE', *, *, #15259, .F. ) ;
#19046 = ORIENTED_EDGE ( 'NONE', *, *, #9789, .F. ) ;
#19047 = DIRECTION ( 'NONE',  ( -1.000000000000000000, 0.000000000000000000, 0.000000000000000000 ) ) ;
#19048 = DIRECTION ( 'NONE',  ( 0.000000000000000000, 0.000000000000000000, 1.000000000000000000 ) ) ;
#19049 = CYLINDRICAL_SURFACE ( 'NONE', #7775, 1.000000000000000888 ) ;
#19050 = DIRECTION ( 'NONE',  ( 0.000000000000000000, 1.000000000000000000, 0.000000000000000000 ) ) ;
#19051 =( NAMED_UNIT ( * ) SI_UNIT ( $, .STERADIAN. ) SOLID_ANGLE_UNIT ( ) );
#19052 = DIRECTION ( 'NONE',  ( 1.000000000000000000, 3.358721889151030981E-15, -1.224646799147353207E-16 ) ) ;
#19053 = CARTESIAN_POINT ( 'NONE',  ( 29.50000000000002132, 69.00000000000000000, 1.500000000000000000 ) ) ;
#19054 = CARTESIAN_POINT ( 'NONE',  ( 23.26716210542296182, -3.307210766252309142, 13.49999999999999822 ) ) ;
#19055 = CARTESIAN_POINT ( 'NONE',  ( 1.824728116533979705, 43.26054587065083012, 41.66679706732590915 ) ) ;
#19056 = CARTESIAN_POINT ( 'NONE',  ( -10.22290649399594642, 41.92645089659918511, 68.06527860057354928 ) ) ;
#19057 = ORIENTED_EDGE ( 'NONE', *, *, #20087, .T. ) ;
#19058 = EDGE_LOOP ( 'NONE', ( #1001, #13303, #20286, #17243, #15596, #18044, #9593, #12306 ) ) ;
#19059 = DIRECTION ( 'NONE',  ( 1.000000000000000000, 0.000000000000000000, 0.000000000000000000 ) ) ;
#19060 = EDGE_CURVE ( 'NONE', #17384, #17645, #1388, .T. ) ;
#19061 = SURFACE_SIDE_STYLE ('',( #20749 ) ) ;
#19062 = DIRECTION ( 'NONE',  ( 0.000000000000000000, 0.000000000000000000, 1.000000000000000000 ) ) ;
#19063 = ORIENTED_EDGE ( 'NONE', *, *, #1696, .T. ) ;
#19064 = ADVANCED_FACE ( 'NONE', ( #22115 ), #16826, .T. ) ;
#19065 = DIRECTION ( 'NONE',  ( 0.000000000000000000, 0.000000000000000000, 1.000000000000000000 ) ) ;
#19066 = VERTEX_POINT ( 'NONE', #18508 ) ;
#19067 = CARTESIAN_POINT ( 'NONE',  ( -9.178906393579158163, 42.46645089659918426, 70.88527860057354246 ) ) ;
#19068 = AXIS2_PLACEMENT_3D ( 'NONE', #20502, #20611, #8644 ) ;
#19069 = CARTESIAN_POINT ( 'NONE',  ( -1.724728116533986721, 42.36054587065083155, 47.70876104995654288 ) ) ;
#19070 = EDGE_LOOP ( 'NONE', ( #4542, #20042, #10400, #2058 ) ) ;
#19071 = DIRECTION ( 'NONE',  ( -0.000000000000000000, -0.000000000000000000, -1.000000000000000000 ) ) ;
#19072 = DIRECTION ( 'NONE',  ( -0.000000000000000000, -1.000000000000000000, -0.000000000000000000 ) ) ;
#19073 = EDGE_CURVE ( 'NONE', #9562, #16208, #4983, .T. ) ;
#19074 = DIRECTION ( 'NONE',  ( -2.107255972849994642E-16, 0.000000000000000000, -1.000000000000000000 ) ) ;
#19075 = DIRECTION ( 'NONE',  ( 0.000000000000000000, 0.000000000000000000, 1.000000000000000000 ) ) ;
#19076 = DIRECTION ( 'NONE',  ( 0.000000000000000000, -1.000000000000000000, -0.000000000000000000 ) ) ;
#19077 = CARTESIAN_POINT ( 'NONE',  ( -30.37540678000427619, -6.000000000000000000, 7.500000000000000000 ) ) ;
#19078 = CYLINDRICAL_SURFACE ( 'NONE', #14881, 1.000000000000000888 ) ;
#19079 = AXIS2_PLACEMENT_3D ( 'NONE', #16264, #9700, #11035 ) ;
#19080 = DIRECTION ( 'NONE',  ( 1.000000000000000000, -0.000000000000000000, -0.000000000000000000 ) ) ;
#19081 = DIRECTION ( 'NONE',  ( 1.000000000000000000, 0.000000000000000000, 0.000000000000000000 ) ) ;
#19082 = CARTESIAN_POINT ( 'NONE',  ( -9.641460742840918030, 32.11873716947361856, 68.00000000000000000 ) ) ;
#19083 = ORIENTED_EDGE ( 'NONE', *, *, #15383, .F. ) ;
#19084 = ORIENTED_EDGE ( 'NONE', *, *, #16843, .F. ) ;
#19085 = DIRECTION ( 'NONE',  ( 1.000000000000000000, 0.000000000000000000, 0.000000000000000000 ) ) ;
#19086 = LINE ( 'NONE', #18986, #14549 ) ;
#19087 = DIRECTION ( 'NONE',  ( 0.000000000000000000, 0.000000000000000000, 1.000000000000000000 ) ) ;
#19088 = ADVANCED_FACE ( 'NONE', ( #6789 ), #17104, .T. ) ;
#19089 = AXIS2_PLACEMENT_3D ( 'NONE', #7739, #21281, #21622 ) ;
#19090 = EDGE_CURVE ( 'NONE', #4254, #18926, #20311, .T. ) ;
#19091 = CARTESIAN_POINT ( 'NONE',  ( -13.75390639357915923, 42.46645089659918426, 70.88527860057354246 ) ) ;
#19092 = ADVANCED_FACE ( 'NONE', ( #15477 ), #1838, .F. ) ;
#19093 = ORIENTED_EDGE ( 'NONE', *, *, #9399, .F. ) ;
#19094 = CARTESIAN_POINT ( 'NONE',  ( -29.69597781366221767, 58.94165929845684815, 70.50000000000000000 ) ) ;
#19095 = ORIENTED_EDGE ( 'NONE', *, *, #11543, .T. ) ;
#19096 = CARTESIAN_POINT ( 'NONE',  ( -1.724728116533986721, 43.31054587065082728, 51.80876104995653719 ) ) ;
#19097 = DIRECTION ( 'NONE',  ( -1.000000000000000000, 0.000000000000000000, -0.000000000000000000 ) ) ;
#19098 = CARTESIAN_POINT ( 'NONE',  ( -15.95292532278785913, -32.61873716947361856, 68.50000000000000000 ) ) ;
#19099 = LINE ( 'NONE', #17627, #12328 ) ;
#19100 = ORIENTED_EDGE ( 'NONE', *, *, #15529, .F. ) ;
#19101 = CARTESIAN_POINT ( 'NONE',  ( 23.04273166366736447, 2.261511273149737100, 13.23427437508501647 ) ) ;
#19102 = CARTESIAN_POINT ( 'NONE',  ( -14.66174975910705136, 0.000000000000000000, 13.50000000000000000 ) ) ;
#19103 = ADVANCED_FACE ( 'NONE', ( #18851 ), #12378, .F. ) ;
#19104 = CARTESIAN_POINT ( 'NONE',  ( -32.23382792203229741, 83.71979900898287497, 13.75000000000000000 ) ) ;
#19105 = DIRECTION ( 'NONE',  ( -0.000000000000000000, -0.000000000000000000, -1.000000000000000000 ) ) ;
#19106 = ORIENTED_EDGE ( 'NONE', *, *, #1138, .F. ) ;
#19107 = CYLINDRICAL_SURFACE ( 'NONE', #176, 0.5000000000000004441 ) ;
#19108 = ORIENTED_EDGE ( 'NONE', *, *, #8859, .F. ) ;
#19109 = LINE ( 'NONE', #20386, #13025 ) ;
#19110 = CARTESIAN_POINT ( 'NONE',  ( -23.02398829872513986, -2.157133568460768647, 7.500000000000000000 ) ) ;
#19111 = ORIENTED_EDGE ( 'NONE', *, *, #4671, .T. ) ;
#19112 = ORIENTED_EDGE ( 'NONE', *, *, #20614, .T. ) ;
#19113 = DIRECTION ( 'NONE',  ( -2.107255972849994642E-16, 0.000000000000000000, -1.000000000000000000 ) ) ;
#19114 = EDGE_CURVE ( 'NONE', #17690, #4912, #10126, .T. ) ;
#19115 = VERTEX_POINT ( 'NONE', #13588 ) ;
#19116 = EDGE_CURVE ( 'NONE', #21318, #1488, #20426, .T. ) ;
#19117 = VERTEX_POINT ( 'NONE', #1726 ) ;
#19118 = CIRCLE ( 'NONE', #20562, 2.000000000000001776 ) ;
#19119 = VECTOR ( 'NONE', #10659, 1000.000000000000000 ) ;
#19120 = ORIENTED_EDGE ( 'NONE', *, *, #4311, .T. ) ;
#19121 = CARTESIAN_POINT ( 'NONE',  ( 1.774728116533973665, 42.31054587065082728, 24.00000000000000000 ) ) ;
#19122 = DIRECTION ( 'NONE',  ( 0.000000000000000000, 0.000000000000000000, 1.000000000000000000 ) ) ;
#19123 = CARTESIAN_POINT ( 'NONE',  ( -27.67540678000428045, 7.839012376739720627E-15, 13.79999999999999893 ) ) ;
#19124 = DIRECTION ( 'NONE',  ( 0.000000000000000000, 0.000000000000000000, -1.000000000000000000 ) ) ;
#19125 = CARTESIAN_POINT ( 'NONE',  ( -29.13662752439705272, 4.700000000000000178, 3.500000000000000000 ) ) ;
#19126 = EDGE_LOOP ( 'NONE', ( #16456, #2759, #14970, #17138, #16050, #2883, #15449, #6927, #7286, #10733 ) ) ;
#19127 = CARTESIAN_POINT ( 'NONE',  ( 29.26786194551793230, 2.777377181973344822, -5.247369108240390601E-15 ) ) ;
#19128 = EDGE_CURVE ( 'NONE', #21291, #21163, #6344, .T. ) ;
#19129 = DIRECTION ( 'NONE',  ( 0.000000000000000000, 0.000000000000000000, 1.000000000000000000 ) ) ;
#19130 = ADVANCED_FACE ( 'NONE', ( #12219, #17600 ), #5656, .T. ) ;
#19131 = DIRECTION ( 'NONE',  ( -1.224646799147353207E-16, -0.000000000000000000, -1.000000000000000000 ) ) ;
#19132 = VECTOR ( 'NONE', #15419, 1000.000000000000000 ) ;
#19133 = VERTEX_POINT ( 'NONE', #7111 ) ;
#19134 = DIRECTION ( 'NONE',  ( 0.000000000000000000, 1.000000000000000000, 0.000000000000000000 ) ) ;
#19135 = DIRECTION ( 'NONE',  ( -0.000000000000000000, 0.000000000000000000, 1.000000000000000000 ) ) ;
#19136 = ORIENTED_EDGE ( 'NONE', *, *, #14451, .T. ) ;
#19137 = EDGE_LOOP ( 'NONE', ( #19684, #20771, #20399, #4442 ) ) ;
#19138 = ORIENTED_EDGE ( 'NONE', *, *, #20907, .T. ) ;
#19139 = CARTESIAN_POINT ( 'NONE',  ( 29.13662752439705272, 5.000000000000000000, 3.799999999999999822 ) ) ;
#19141 = EDGE_CURVE ( 'NONE', #3486, #9143, #20756, .T. ) ;
#19140 =( NAMED_UNIT ( * ) PLANE_ANGLE_UNIT ( ) SI_UNIT ( $, .RADIAN. ) );
#19142 = ORIENTED_EDGE ( 'NONE', *, *, #19394, .F. ) ;
#19143 = CIRCLE ( 'NONE', #9848, 0.2500000000000002220 ) ;
#19144 = CARTESIAN_POINT ( 'NONE',  ( 23.02398829872513986, -3.004888651530553290, 13.74579066068641708 ) ) ;
#19145 = ORIENTED_EDGE ( 'NONE', *, *, #14292, .T. ) ;
#19146 = CIRCLE ( 'NONE', #8089, 0.05000000000000143219 ) ;
#19147 = CIRCLE ( 'NONE', #2702, 0.2999999999999999334 ) ;
#19148 = EDGE_LOOP ( 'NONE', ( #14369, #2874, #21710, #9916 ) ) ;
#19149 = DIRECTION ( 'NONE',  ( 0.000000000000000000, 0.000000000000000000, 1.000000000000000000 ) ) ;
#19150 = DIRECTION ( 'NONE',  ( -0.000000000000000000, -1.000000000000000000, -0.000000000000000000 ) ) ;
#19151 = CARTESIAN_POINT ( 'NONE',  ( -23.36078716634399655, 44.83461903493144973, 13.74999999999999822 ) ) ;
#19152 = DIRECTION ( 'NONE',  ( 0.000000000000000000, 1.000000000000000000, -0.000000000000000000 ) ) ;
#19153 = DIRECTION ( 'NONE',  ( -1.094601647044990554E-16, -1.000000000000000000, 0.000000000000000000 ) ) ;
#19154 = DIRECTION ( 'NONE',  ( 0.000000000000000000, 0.000000000000000000, -1.000000000000000000 ) ) ;
#19155 = EDGE_CURVE ( 'NONE', #1327, #6378, #13516, .T. ) ;
#19156 = LINE ( 'NONE', #3839, #9095 ) ;
#19157 = DIRECTION ( 'NONE',  ( 0.000000000000000000, 0.000000000000000000, 1.000000000000000000 ) ) ;
#19158 = AXIS2_PLACEMENT_3D ( 'NONE', #21396, #5953, #4375 ) ;
#19159 = AXIS2_PLACEMENT_3D ( 'NONE', #2733, #6114, #4523 ) ;
#19160 = CIRCLE ( 'NONE', #8443, 0.05000000000000143219 ) ;
#19161 = CARTESIAN_POINT ( 'NONE',  ( -14.97529860451076722, -51.91950568661984278, 13.84831215707030516 ) ) ;
#19162 = TOROIDAL_SURFACE ( 'NONE', #16282, 1.000000000000000000, 0.5000000000000000000 ) ;
#19163 = ORIENTED_EDGE ( 'NONE', *, *, #5348, .F. ) ;
#19164 = ORIENTED_EDGE ( 'NONE', *, *, #3097, .F. ) ;
#19165 = DIRECTION ( 'NONE',  ( 0.000000000000000000, 0.000000000000000000, 1.000000000000000000 ) ) ;
#19166 = CARTESIAN_POINT ( 'NONE',  ( -30.79999999999999005, 85.00000000000000000, 2.571758278209449353E-16 ) ) ;
#19167 = ORIENTED_EDGE ( 'NONE', *, *, #5117, .F. ) ;
#19168 = EDGE_LOOP ( 'NONE', ( #1543, #11761, #18609, #19579, #3573, #3188, #20508, #3693, #10056, #17127 ) ) ;
#19169 = EDGE_CURVE ( 'NONE', #22072, #11729, #19291, .T. ) ;
#19170 = AXIS2_PLACEMENT_3D ( 'NONE', #21228, #7581, #5573 ) ;
#19171 = CIRCLE ( 'NONE', #10939, 0.2500000000000002220 ) ;
#19172 = VECTOR ( 'NONE', #11742, 1000.000000000000000 ) ;
#19173 = DIRECTION ( 'NONE',  ( -0.000000000000000000, 0.000000000000000000, 1.000000000000000000 ) ) ;
#19174 = DIRECTION ( 'NONE',  ( 0.000000000000000000, -0.000000000000000000, -1.000000000000000000 ) ) ;
#19175 = AXIS2_PLACEMENT_3D ( 'NONE', #22069, #4724, #3035 ) ;
#19176 = ORIENTED_EDGE ( 'NONE', *, *, #16528, .F. ) ;
#19177 = DIRECTION ( 'NONE',  ( -0.000000000000000000, -1.000000000000000000, 0.000000000000000000 ) ) ;
#19178 = DIRECTION ( 'NONE',  ( 0.000000000000000000, 0.000000000000000000, -1.000000000000000000 ) ) ;
#19179 = EDGE_CURVE ( 'NONE', #6175, #8145, #9601, .T. ) ;
#19180 = ADVANCED_FACE ( 'NONE', ( #8888 ), #21090, .F. ) ;
#19181 = CARTESIAN_POINT ( 'NONE',  ( 1.724728116533979616, 42.31054587065082728, 49.71679706732589921 ) ) ;
#19182 = CARTESIAN_POINT ( 'NONE',  ( -29.37540678000427619, -6.000000000000000000, 7.500000000000000000 ) ) ;
#19183 = CARTESIAN_POINT ( 'NONE',  ( 0.000000000000000000, -69.04634676501045476, 3.799999999999999822 ) ) ;
#19184 = DIRECTION ( 'NONE',  ( 0.000000000000000000, 0.000000000000000000, 1.000000000000000000 ) ) ;
#19185 = VERTEX_POINT ( 'NONE', #10677 ) ;
#19186 = CARTESIAN_POINT ( 'NONE',  ( 28.71290943744531177, -6.649236572130504896, 13.47739020623642325 ) ) ;
#19187 = DIRECTION ( 'NONE',  ( 0.000000000000000000, 0.000000000000000000, 1.000000000000000000 ) ) ;
#19188 = TOROIDAL_SURFACE ( 'NONE', #11315, 2.767785046117003489, 0.2500000000000000000 ) ;
#19189 = ORIENTED_EDGE ( 'NONE', *, *, #9234, .F. ) ;
#19190 = AXIS2_PLACEMENT_3D ( 'NONE', #16878, #20140, #6611 ) ;
#19191 = CIRCLE ( 'NONE', #232, 0.05000000000000143219 ) ;
#19192 = ORIENTED_EDGE ( 'NONE', *, *, #7447, .F. ) ;
#19193 = ORIENTED_EDGE ( 'NONE', *, *, #21974, .F. ) ;
#19194 = DIRECTION ( 'NONE',  ( 0.000000000000000000, 0.000000000000000000, 1.000000000000000000 ) ) ;
#19195 = DIRECTION ( 'NONE',  ( 0.000000000000000000, 1.000000000000000000, 0.000000000000000000 ) ) ;
#19196 = DIRECTION ( 'NONE',  ( 0.000000000000000000, 0.000000000000000000, 1.000000000000000000 ) ) ;
#19197 = CIRCLE ( 'NONE', #20991, 0.2999999999999999334 ) ;
#19198 = EDGE_LOOP ( 'NONE', ( #13514, #8001, #16344, #13095 ) ) ;
#19199 = DIRECTION ( 'NONE',  ( -1.000000000000000000, 0.000000000000000000, 0.000000000000000000 ) ) ;
#19200 = AXIS2_PLACEMENT_3D ( 'NONE', #18985, #3547, #5115 ) ;
#19201 = EDGE_CURVE ( 'NONE', #11697, #620, #17044, .T. ) ;
#19202 = ORIENTED_EDGE ( 'NONE', *, *, #6815, .T. ) ;
#19203 = LINE ( 'NONE', #19094, #20785 ) ;
#19204 = ORIENTED_EDGE ( 'NONE', *, *, #21113, .T. ) ;
#19205 = DIRECTION ( 'NONE',  ( -6.123233995736764803E-17, 0.000000000000000000, 1.000000000000000000 ) ) ;
#19206 = CARTESIAN_POINT ( 'NONE',  ( -1.774728116533986544, 43.26054587065083012, 39.80876104995653719 ) ) ;
#19207 = AXIS2_PLACEMENT_3D ( 'NONE', #8834, #16990, #10510 ) ;
#19208 = VECTOR ( 'NONE', #12179, 1000.000000000000000 ) ;
#19209 = DIRECTION ( 'NONE',  ( 0.000000000000000000, 1.000000000000000000, 0.000000000000000000 ) ) ;
#19210 = CYLINDRICAL_SURFACE ( 'NONE', #16623, 0.05000000000000143219 ) ;
#19211 = EDGE_LOOP ( 'NONE', ( #17114, #6562, #16582, #19887 ) ) ;
#19212 = LINE ( 'NONE', #12584, #18432 ) ;
#19213 = DIRECTION ( 'NONE',  ( 1.000000000000000000, 0.000000000000000000, -0.000000000000000000 ) ) ;
#19214 = EDGE_CURVE ( 'NONE', #2467, #18467, #12428, .T. ) ;
#19215 = EDGE_CURVE ( 'NONE', #2805, #15492, #10269, .T. ) ;
#19216 = EDGE_CURVE ( 'NONE', #11776, #8252, #14014, .T. ) ;
#19217 = AXIS2_PLACEMENT_3D ( 'NONE', #11345, #16491, #14700 ) ;
#19218 = CARTESIAN_POINT ( 'NONE',  ( 27.37540678000428684, -36.74634676501047181, 13.79999999999999893 ) ) ;
#19219 = CARTESIAN_POINT ( 'NONE',  ( -23.04273156199908357, -2.261510999192740901, 13.19999999999999929 ) ) ;
#19220 = VERTEX_POINT ( 'NONE', #5866 ) ;
#19221 = DIRECTION ( 'NONE',  ( 0.000000000000000000, 0.000000000000000000, 1.000000000000000000 ) ) ;
#19222 = EDGE_CURVE ( 'NONE', #6732, #21679, #13102, .T. ) ;
#19223 = VECTOR ( 'NONE', #965, 1000.000000000000000 ) ;
#19224 = ORIENTED_EDGE ( 'NONE', *, *, #4621, .F. ) ;
#19225 = CARTESIAN_POINT ( 'NONE',  ( 23.04273156199908357, -2.261510999192740901, 7.500000000000000000 ) ) ;
#19226 = LINE ( 'NONE', #17540, #5961 ) ;
#19227 = VERTEX_POINT ( 'NONE', #366 ) ;
#19228 = ORIENTED_EDGE ( 'NONE', *, *, #13382, .T. ) ;
#19229 = CARTESIAN_POINT ( 'NONE',  ( -17.95292532278785913, 50.11873716947361856, 68.00000000000000000 ) ) ;
#19230 = CIRCLE ( 'NONE', #3864, 0.5999999999999998668 ) ;
#19231 = AXIS2_PLACEMENT_3D ( 'NONE', #13521, #20364, #17546 ) ;
#19232 = VERTEX_POINT ( 'NONE', #13905 ) ;
#19233 = ADVANCED_FACE ( 'NONE', ( #9097 ), #5536, .F. ) ;
#19234 = AXIS2_PLACEMENT_3D ( 'NONE', #19593, #10305, #11848 ) ;
#19235 = ORIENTED_EDGE ( 'NONE', *, *, #16908, .T. ) ;
#19236 = CIRCLE ( 'NONE', #3520, 0.5000000000000004441 ) ;
#19237 = AXIS2_PLACEMENT_3D ( 'NONE', #15503, #13820, #4093 ) ;
#19238 = ORIENTED_EDGE ( 'NONE', *, *, #4624, .T. ) ;
#19239 = DIRECTION ( 'NONE',  ( 1.000000000000000000, 0.000000000000000000, 0.000000000000000000 ) ) ;
#19240 = CARTESIAN_POINT ( 'NONE',  ( 1.724728116533979616, 43.26054587065083012, 35.70876104995653577 ) ) ;
#19241 = DIRECTION ( 'NONE',  ( 0.000000000000000000, 0.000000000000000000, 1.000000000000000000 ) ) ;
#19242 = ADVANCED_FACE ( 'NONE', ( #7322 ), #19188, .T. ) ;
#19243 = ADVANCED_FACE ( 'NONE', ( #12316 ), #8999, .F. ) ;
#19244 = ORIENTED_EDGE ( 'NONE', *, *, #20408, .F. ) ;
#19245 = AXIS2_PLACEMENT_3D ( 'NONE', #9210, #694, #7985 ) ;
#19246 = CIRCLE ( 'NONE', #1371, 0.05000000000000143219 ) ;
#19247 = DIRECTION ( 'NONE',  ( 0.000000000000000000, 1.000000000000000000, 0.000000000000000000 ) ) ;
#19248 = ADVANCED_FACE ( 'NONE', ( #17695 ), #2378, .T. ) ;
#19249 = CARTESIAN_POINT ( 'NONE',  ( -25.37540678000427263, 63.74634676501045050, 3.799999999999999822 ) ) ;
#19250 = VECTOR ( 'NONE', #14966, 1000.000000000000000 ) ;
#19251 = CARTESIAN_POINT ( 'NONE',  ( -29.13662752439705272, 0.000000000000000000, 13.19999999999999929 ) ) ;
#19252 = CIRCLE ( 'NONE', #18167, 0.05000000000000143219 ) ;
#19253 = AXIS2_PLACEMENT_3D ( 'NONE', #5508, #666, #219 ) ;
#19254 = CIRCLE ( 'NONE', #12805, 0.2500000000000002220 ) ;
#19255 = ORIENTED_EDGE ( 'NONE', *, *, #16359, .T. ) ;
#19256 = DIRECTION ( 'NONE',  ( 0.000000000000000000, 0.000000000000000000, 1.000000000000000000 ) ) ;
#19257 = ORIENTED_EDGE ( 'NONE', *, *, #15085, .F. ) ;
#19258 = ORIENTED_EDGE ( 'NONE', *, *, #3629, .F. ) ;
#19259 = DIRECTION ( 'NONE',  ( -0.000000000000000000, 1.000000000000000000, 0.000000000000000000 ) ) ;
#19260 = ORIENTED_EDGE ( 'NONE', *, *, #165, .F. ) ;
#19261 = ORIENTED_EDGE ( 'NONE', *, *, #10052, .F. ) ;
#19262 = AXIS2_PLACEMENT_3D ( 'NONE', #13831, #19105, #8814 ) ;
#19263 = ADVANCED_FACE ( 'NONE', ( #806 ), #18108, .F. ) ;
#19264 = CARTESIAN_POINT ( 'NONE',  ( 23.02398829872513986, -3.395586890286260484, 13.79999998301280328 ) ) ;
#19265 = ORIENTED_EDGE ( 'NONE', *, *, #126, .T. ) ;
#19266 = AXIS2_PLACEMENT_3D ( 'NONE', #4069, #9852, #19296 ) ;
#19267 = ORIENTED_EDGE ( 'NONE', *, *, #731, .F. ) ;
#19268 = CIRCLE ( 'NONE', #18730, 0.05000000000000143219 ) ;
#19269 = LINE ( 'NONE', #3945, #13060 ) ;
#19270 = DIRECTION ( 'NONE',  ( -1.000000000000000000, -0.000000000000000000, 2.388292521039847891E-16 ) ) ;
#19271 = DIRECTION ( 'NONE',  ( -0.000000000000000000, -0.000000000000000000, -1.000000000000000000 ) ) ;
#19272 = FILL_AREA_STYLE_COLOUR ( '', #26 ) ;
#19273 = EDGE_CURVE ( 'NONE', #21435, #17559, #9668, .T. ) ;
#19274 = CARTESIAN_POINT ( 'NONE',  ( -23.06501889853218401, 2.381465418138768886, 13.31529126727256873 ) ) ;
#19275 = DIRECTION ( 'NONE',  ( -1.000000000000000000, 0.000000000000000000, 0.000000000000000000 ) ) ;
#19276 = DIRECTION ( 'NONE',  ( 0.000000000000000000, -1.000000000000000000, 0.000000000000000000 ) ) ;
#19277 = DIRECTION ( 'NONE',  ( 1.000000000000000000, 0.000000000000000000, 0.000000000000000000 ) ) ;
#19278 = DIRECTION ( 'NONE',  ( 0.000000000000000000, 0.000000000000000000, 1.000000000000000000 ) ) ;
#19279 = AXIS2_PLACEMENT_3D ( 'NONE', #19452, #12507, #10626 ) ;
#19280 =( BOUNDED_SURFACE ( )  B_SPLINE_SURFACE ( 3, 2, ( 
 ( #9544, #18151, #16360 ),
 ( #7884, #14679, #21535 ),
 ( #4500, #18265, #11321 ),
 ( #9320, #2838, #1241 ),
 ( #8095, #6433, #13229 ),
 ( #17814, #10212, #10333 ),
 ( #1581, #8211, #15022 ),
 ( #11764, #18481, #16915 ) ),
 .UNSPECIFIED., .F., .F., .T. ) 
 B_SPLINE_SURFACE_WITH_KNOTS ( ( 4, 2, 2, 4 ),
 ( 3, 3 ),
 ( -1.707618421664669484E-18, 0.0004639257417130348096, 0.0006958886125695531088, 0.0009278514834260713539 ),
 ( 0.000000000000000000, 1.000000000000000000 ),
 .UNSPECIFIED. ) 
 GEOMETRIC_REPRESENTATION_ITEM ( )  RATIONAL_B_SPLINE_SURFACE ( (
 ( 1.000000000000000000, 0.6123724356957929160, 1.000000000000000000),
 ( 1.000000000000000000, 0.6127303078017206639, 1.000000000000000000),
 ( 1.000000000000000000, 0.6153173443167760936, 1.000000000000000000),
 ( 1.000000000000000000, 0.6312737947278392880, 1.000000000000000000),
 ( 1.000000000000000000, 0.6386439821288609764, 1.000000000000000000),
 ( 1.000000000000000000, 0.6635434878155272997, 1.000000000000000000),
 ( 1.000000000000000000, 0.6820474757551056033, 1.000000000000000000),
 ( 1.000000000000000000, 0.7071067811865495711, 1.000000000000000000) ) ) 
 REPRESENTATION_ITEM ( '' )  SURFACE ( )  );
#19281 = ORIENTED_EDGE ( 'NONE', *, *, #15498, .F. ) ;
#19282 = DIRECTION ( 'NONE',  ( 0.000000000000000000, 0.000000000000000000, 1.000000000000000000 ) ) ;
#19283 = CARTESIAN_POINT ( 'NONE',  ( 1.824728116533979705, 43.31054587065082728, 37.66679706732590915 ) ) ;
#19284 = ORIENTED_EDGE ( 'NONE', *, *, #4944, .F. ) ;
#19285 = ORIENTED_EDGE ( 'NONE', *, *, #9538, .T. ) ;
#19286 = ORIENTED_EDGE ( 'NONE', *, *, #14856, .F. ) ;
#19287 = EDGE_CURVE ( 'NONE', #2269, #20918, #5686, .T. ) ;
#19288 = EDGE_CURVE ( 'NONE', #9360, #8599, #4628, .T. ) ;
#19289 = AXIS2_PLACEMENT_3D ( 'NONE', #7328, #14121, #2166 ) ;
#19290 = CIRCLE ( 'NONE', #5738, 0.2999999999999947153 ) ;
#19291 = LINE ( 'NONE', #12648, #14225 ) ;
#19292 = AXIS2_PLACEMENT_3D ( 'NONE', #20880, #15496, #1859 ) ;
#19293 = CYLINDRICAL_SURFACE ( 'NONE', #20239, 0.04999999999999991257 ) ;
#19294 = VERTEX_POINT ( 'NONE', #14567 ) ;
#19295 = CARTESIAN_POINT ( 'NONE',  ( 25.37540678000426908, 36.74634676501047181, 13.50000000000000000 ) ) ;
#19296 = DIRECTION ( 'NONE',  ( -1.000000000000000000, -2.312964634635729960E-14, 0.000000000000000000 ) ) ;
#19297 = DIRECTION ( 'NONE',  ( -0.000000000000000000, -0.000000000000000000, -1.000000000000000000 ) ) ;
#19298 = DIRECTION ( 'NONE',  ( -0.000000000000000000, -1.000000000000000000, -0.000000000000000000 ) ) ;
#19299 = CYLINDRICAL_SURFACE ( 'NONE', #21153, 0.3000000000000003775 ) ;
#19300 = DIRECTION ( 'NONE',  ( 1.000000000000000000, -0.000000000000000000, -0.000000000000000000 ) ) ;
#19301 = DIRECTION ( 'NONE',  ( -1.000000000000000000, 0.000000000000000000, -0.000000000000000000 ) ) ;
#19302 = LINE ( 'NONE', #15708, #22065 ) ;
#19303 = EDGE_CURVE ( 'NONE', #17257, #11459, #18157, .T. ) ;
#19304 = ORIENTED_EDGE ( 'NONE', *, *, #10910, .F. ) ;
#19305 = ORIENTED_EDGE ( 'NONE', *, *, #2365, .F. ) ;
#19306 = ORIENTED_EDGE ( 'NONE', *, *, #17234, .F. ) ;
#19307 = FACE_OUTER_BOUND ( 'NONE', #19929, .T. ) ;
#19308 = AXIS2_PLACEMENT_3D ( 'NONE', #14808, #16386, #21329 ) ;
#19309 = DIRECTION ( 'NONE',  ( 1.000000000000000000, 0.000000000000000000, 0.000000000000000000 ) ) ;
#19310 = ORIENTED_EDGE ( 'NONE', *, *, #520, .T. ) ;
#19311 =( GEOMETRIC_REPRESENTATION_CONTEXT ( 3 ) GLOBAL_UNCERTAINTY_ASSIGNED_CONTEXT ( ( #4620 ) ) GLOBAL_UNIT_ASSIGNED_CONTEXT ( ( #13765, #20625, #18945 ) ) REPRESENTATION_CONTEXT ( 'NONE', 'WORKASPACE' ) );
#19312 = CYLINDRICAL_SURFACE ( 'NONE', #1340, 0.04999999999999991257 ) ;
#19313 = EDGE_CURVE ( 'NONE', #14178, #4942, #15491, .T. ) ;
#19314 = ORIENTED_EDGE ( 'NONE', *, *, #20680, .T. ) ;
#19315 = CARTESIAN_POINT ( 'NONE',  ( -9.178906393579158163, 42.46645089659918426, 67.85468508031152624 ) ) ;
#19316 = DIRECTION ( 'NONE',  ( 0.000000000000000000, 0.000000000000000000, 1.000000000000000000 ) ) ;
#19317 = ORIENTED_EDGE ( 'NONE', *, *, #5973, .F. ) ;
#19318 = DIRECTION ( 'NONE',  ( 0.000000000000000000, -1.000000000000000000, 0.000000000000000000 ) ) ;
#19319 = CARTESIAN_POINT ( 'NONE',  ( 15.95292532278785913, -34.11873716947361856, 68.00000000000000000 ) ) ;
#19320 = CARTESIAN_POINT ( 'NONE',  ( -9.178906393579158163, 42.46645089659918426, 68.75385983073485363 ) ) ;
#19321 = FACE_OUTER_BOUND ( 'NONE', #5896, .T. ) ;
#19322 = ORIENTED_EDGE ( 'NONE', *, *, #4944, .T. ) ;
#19323 = CARTESIAN_POINT ( 'NONE',  ( -31.50000000000002132, 72.00000000000001421, 3.500000000000000000 ) ) ;
#19324 = FACE_OUTER_BOUND ( 'NONE', #3155, .T. ) ;
#19325 = AXIS2_PLACEMENT_3D ( 'NONE', #784, #7731, #550 ) ;
#19326 = TOROIDAL_SURFACE ( 'NONE', #9688, 0.2999999999999999889, 0.2999999999999999889 ) ;
#19327 = CARTESIAN_POINT ( 'NONE',  ( 31.50000000000002132, -71.00000000000001421, 3.500000000000000000 ) ) ;
#19328 = DIRECTION ( 'NONE',  ( 1.000000000000000000, 0.000000000000000000, 0.000000000000000000 ) ) ;
#19329 = ORIENTED_EDGE ( 'NONE', *, *, #3847, .T. ) ;
#19330 = DIRECTION ( 'NONE',  ( 0.000000000000000000, 0.000000000000000000, 1.000000000000000000 ) ) ;
#19331 = EDGE_CURVE ( 'NONE', #20195, #20211, #7410, .T. ) ;
#19332 = EDGE_LOOP ( 'NONE', ( #21256, #8164, #1044, #14395 ) ) ;
#19333 = DIRECTION ( 'NONE',  ( 0.000000000000000000, 0.000000000000000000, 1.000000000000000000 ) ) ;
#19334 = CARTESIAN_POINT ( 'NONE',  ( -4.127054932750482408, -32.93424481021354921, 42.50000000000000000 ) ) ;
#19335 = ORIENTED_EDGE ( 'NONE', *, *, #8438, .T. ) ;
#19336 = VERTEX_POINT ( 'NONE', #908 ) ;
#19337 = CARTESIAN_POINT ( 'NONE',  ( 1.724728116533979616, 42.31054587065082728, 31.75876104995653648 ) ) ;
#19338 = CARTESIAN_POINT ( 'NONE',  ( -15.21174975910705207, 51.61873716947361856, 14.00000000000000000 ) ) ;
#19339 = ORIENTED_EDGE ( 'NONE', *, *, #21239, .F. ) ;
#19340 = EDGE_CURVE ( 'NONE', #19185, #15364, #9431, .T. ) ;
#19341 = ADVANCED_FACE ( 'NONE', ( #10997, #6094 ), #11099, .T. ) ;
#19342 = AXIS2_PLACEMENT_3D ( 'NONE', #5157, #22059, #6739 ) ;
#19343 = ADVANCED_FACE ( 'NONE', ( #19838 ), #17924, .F. ) ;
#19344 = ORIENTED_EDGE ( 'NONE', *, *, #7467, .F. ) ;
#19345 = VERTEX_POINT ( 'NONE', #13109 ) ;
#19346 = DIRECTION ( 'NONE',  ( 0.000000000000000000, -1.000000000000000000, 0.000000000000000000 ) ) ;
#19347 = CARTESIAN_POINT ( 'NONE',  ( 1.724728116533979616, 42.36054587065083155, 27.75876104995654003 ) ) ;
#19348 = CARTESIAN_POINT ( 'NONE',  ( -1.824728116533986810, 43.26054587065083012, 39.80876104995653719 ) ) ;
#19349 = VECTOR ( 'NONE', #11904, 1000.000000000000000 ) ;
#19350 = VECTOR ( 'NONE', #4185, 1000.000000000000000 ) ;
#19351 = CARTESIAN_POINT ( 'NONE',  ( -9.178906393579156386, 42.46645089659917716, 70.50000000000000000 ) ) ;
#19352 = ORIENTED_EDGE ( 'NONE', *, *, #8129, .F. ) ;
#19353 = CARTESIAN_POINT ( 'NONE',  ( -1.824728116533986810, 42.36054587065083155, 53.76679706732590347 ) ) ;
#19354 = ADVANCED_FACE ( 'NONE', ( #11205 ), #19280, .F. ) ;
#19355 = CARTESIAN_POINT ( 'NONE',  ( 28.57540678000427548, 63.74634676501045050, 13.19999999999999929 ) ) ;
#19356 = DIRECTION ( 'NONE',  ( 0.000000000000000000, 0.000000000000000000, 1.000000000000000000 ) ) ;
#19357 = ORIENTED_EDGE ( 'NONE', *, *, #307, .T. ) ;
#19358 = CARTESIAN_POINT ( 'NONE',  ( 14.71174975910705740, 51.61873716947361856, 14.00000000000000000 ) ) ;
#19359 = VERTEX_POINT ( 'NONE', #6643 ) ;
#19360 = CIRCLE ( 'NONE', #17204, 0.5000000000000004441 ) ;
#19361 = VERTEX_POINT ( 'NONE', #15228 ) ;
#19362 = ORIENTED_EDGE ( 'NONE', *, *, #13854, .T. ) ;
#19363 = CARTESIAN_POINT ( 'NONE',  ( -32.23382792203229741, 83.71979900898287497, 13.75000000000000000 ) ) ;
#19364 = ITEM_DEFINED_TRANSFORMATION ( 'NONE', 'NONE', #19068,  #17493 ) ;
#19365 = EDGE_CURVE ( 'NONE', #2085, #8381, #16688, .T. ) ;
#19366 = CIRCLE ( 'NONE', #6510, 0.04999999999999991257 ) ;
#19367 = ORIENTED_EDGE ( 'NONE', *, *, #19386, .F. ) ;
#19368 = VECTOR ( 'NONE', #1666, 1000.000000000000000 ) ;
#19369 = EDGE_CURVE ( 'NONE', #18664, #10231, #1728, .T. ) ;
#19370 = VERTEX_POINT ( 'NONE', #8415 ) ;
#19371 = ADVANCED_FACE ( 'NONE', ( #17020 ), #22084, .T. ) ;
#19372 = CARTESIAN_POINT ( 'NONE',  ( 23.06501889853218401, -2.381465418138775103, 13.31529126727256873 ) ) ;
#19373 = ORIENTED_EDGE ( 'NONE', *, *, #20643, .T. ) ;
#19374 = PLANE ( 'NONE',  #10031 ) ;
#19375 = CYLINDRICAL_SURFACE ( 'NONE', #7371, 0.04999999999999991257 ) ;
#19376 = CARTESIAN_POINT ( 'NONE',  ( 1.724728116533979616, 43.31054587065082728, 35.80876104995653009 ) ) ;
#19377 = FACE_OUTER_BOUND ( 'NONE', #1262, .T. ) ;
#19378 = CARTESIAN_POINT ( 'NONE',  ( 33.19999999999999574, 84.70000000000001705, 1.500000000000004219 ) ) ;
#19379 = AXIS2_PLACEMENT_3D ( 'NONE', #9522, #4380, #9753 ) ;
#19380 = EDGE_CURVE ( 'NONE', #21635, #9395, #4958, .T. ) ;
#19381 = CARTESIAN_POINT ( 'NONE',  ( -3.127054932750481964, 32.61873716947361856, 68.00000000000000000 ) ) ;
#19382 = AXIS2_PLACEMENT_3D ( 'NONE', #10621, #8948, #14399 ) ;
#19383 = FACE_OUTER_BOUND ( 'NONE', #4193, .T. ) ;
#19384 = DIRECTION ( 'NONE',  ( 1.038507728162729222E-16, 1.000000000000000000, -1.271805165184275985E-32 ) ) ;
#19385 = DIRECTION ( 'NONE',  ( 1.000000000000000000, 0.000000000000000000, 0.000000000000000000 ) ) ;
#19386 = EDGE_CURVE ( 'NONE', #17384, #15401, #5069, .T. ) ;
#19387 = ORIENTED_EDGE ( 'NONE', *, *, #22021, .F. ) ;
#19388 = ORIENTED_EDGE ( 'NONE', *, *, #18728, .T. ) ;
#19389 = DIRECTION ( 'NONE',  ( 0.000000000000000000, 1.000000000000000000, 0.000000000000000000 ) ) ;
#19390 = AXIS2_PLACEMENT_3D ( 'NONE', #15464, #1704, #16809 ) ;
#19391 = ORIENTED_EDGE ( 'NONE', *, *, #1610, .T. ) ;
#19392 = B_SPLINE_CURVE_WITH_KNOTS ( 'NONE', 3,
 ( #2399, #12338, #10697, #17718, #3985, #13923 ),
 .UNSPECIFIED., .F., .F.,
 ( 4, 2, 4 ),
 ( 0.000000000000000000, 0.0002343434414548649890, 0.0004686868829097299780 ),
 .UNSPECIFIED. ) ;
#19393 = ORIENTED_EDGE ( 'NONE', *, *, #15229, .F. ) ;
#19394 = EDGE_CURVE ( 'NONE', #16467, #8942, #3829, .T. ) ;
#19395 = FACE_OUTER_BOUND ( 'NONE', #2401, .T. ) ;
#19396 = ORIENTED_EDGE ( 'NONE', *, *, #5124, .T. ) ;
#19397 = CARTESIAN_POINT ( 'NONE',  ( -15.21174975910705207, 52.11873716947361856, 14.00000000000000000 ) ) ;
#19398 = CARTESIAN_POINT ( 'NONE',  ( 23.04273156199909778, 2.261510999192739124, 13.22936009151389669 ) ) ;
#19399 = DIRECTION ( 'NONE',  ( 0.000000000000000000, -1.000000000000000000, 0.000000000000000000 ) ) ;
#19400 = CARTESIAN_POINT ( 'NONE',  ( 15.14085429618050682, 52.10286008412593617, 13.87499998596578976 ) ) ;
#19401 = CARTESIAN_POINT ( 'NONE',  ( -14.90262739788948920, 52.32122552996406739, 13.50000000000000000 ) ) ;
#19402 = DIRECTION ( 'NONE',  ( 0.000000000000000000, 0.000000000000000000, -1.000000000000000000 ) ) ;
#19403 = EDGE_CURVE ( 'NONE', #12457, #17212, #128, .T. ) ;
#19404 = EDGE_LOOP ( 'NONE', ( #14323, #779, #1508, #16321 ) ) ;
#19405 = FACE_OUTER_BOUND ( 'NONE', #18023, .T. ) ;
#19406 = FACE_OUTER_BOUND ( 'NONE', #10925, .T. ) ;
#19407 = ADVANCED_FACE ( 'NONE', ( #6979 ), #1698, .T. ) ;
#19408 = DIRECTION ( 'NONE',  ( 1.000000000000000000, 0.000000000000000000, 0.000000000000000000 ) ) ;
#19409 = ADVANCED_FACE ( 'NONE', ( #9877 ), #13666, .T. ) ;
#19410 = ORIENTED_EDGE ( 'NONE', *, *, #5844, .F. ) ;
#19411 = CARTESIAN_POINT ( 'NONE',  ( -4.127054932750482408, 33.43424481021354921, 68.50000000000000000 ) ) ;
#19412 = DIRECTION ( 'NONE',  ( -1.000000000000000000, -0.000000000000000000, -0.000000000000000000 ) ) ;
#19413 = VERTEX_POINT ( 'NONE', #18369 ) ;
#19414 = DIRECTION ( 'NONE',  ( 1.000000000000000000, 0.000000000000000000, 0.000000000000000000 ) ) ;
#19415 = EDGE_LOOP ( 'NONE', ( #10508, #18354, #15744, #5876 ) ) ;
#19416 =( GEOMETRIC_REPRESENTATION_CONTEXT ( 3 ) GLOBAL_UNCERTAINTY_ASSIGNED_CONTEXT ( ( #15645 ) ) GLOBAL_UNIT_ASSIGNED_CONTEXT ( ( #12874, #6300, #1353 ) ) REPRESENTATION_CONTEXT ( 'NONE', 'WORKASPACE' ) );
#19417 = FACE_OUTER_BOUND ( 'NONE', #18528, .T. ) ;
#19418 = DIRECTION ( 'NONE',  ( 1.000000000000000000, -0.000000000000000000, 0.000000000000000000 ) ) ;
#19419 = CARTESIAN_POINT ( 'NONE',  ( -28.57540678000427548, -6.776800961815481195, 13.50000000000000000 ) ) ;
#19420 = CARTESIAN_POINT ( 'NONE',  ( -1.824728116533986810, 43.31054587065082728, 27.70876104995653577 ) ) ;
#19421 = PRODUCT_DEFINITION ( 'UNKNOWN', '', #490, #8412 ) ;
#19422 = DIRECTION ( 'NONE',  ( -1.000000000000000000, 0.000000000000000000, 0.000000000000000000 ) ) ;
#19423 = DIRECTION ( 'NONE',  ( 0.000000000000000000, 0.000000000000000000, 1.000000000000000000 ) ) ;
#19424 = ORIENTED_EDGE ( 'NONE', *, *, #17518, .F. ) ;
#19425 = CARTESIAN_POINT ( 'NONE',  ( -1.824728116533986810, 43.26054587065083012, 35.80876104995653009 ) ) ;
#19426 = DIRECTION ( 'NONE',  ( 0.1868663427273192512, 0.9823853469773029534, 0.000000000000000000 ) ) ;
#19427 = DIRECTION ( 'NONE',  ( -1.000000000000000000, 0.000000000000000000, 0.000000000000000000 ) ) ;
#19428 = DIRECTION ( 'NONE',  ( 0.000000000000000000, 0.000000000000000000, -1.000000000000000000 ) ) ;
#19429 = VERTEX_POINT ( 'NONE', #10105 ) ;
#19430 = CARTESIAN_POINT ( 'NONE',  ( -8.378839169841056034, 43.00645089659919051, 68.06527860057354928 ) ) ;
#19431 = ADVANCED_FACE ( 'NONE', ( #17141 ), #3277, .T. ) ;
#19432 = VERTEX_POINT ( 'NONE', #20070 ) ;
#19433 = LINE ( 'NONE', #10188, #521 ) ;
#19434 = CARTESIAN_POINT ( 'NONE',  ( 26.37540678000427619, 10.94079601157914539, 13.79999999999999893 ) ) ;
#19435 = PRODUCT_DEFINITION_FORMATION_WITH_SPECIFIED_SOURCE ( 'ANY', '', #9655, .NOT_KNOWN. ) ;
#19436 = ADVANCED_FACE ( 'NONE', ( #11542 ), #3047, .F. ) ;
#19437 = ORIENTED_EDGE ( 'NONE', *, *, #18114, .F. ) ;
#19438 = ORIENTED_EDGE ( 'NONE', *, *, #16616, .F. ) ;
#19439 = CYLINDRICAL_SURFACE ( 'NONE', #11699, 0.2500000000000002220 ) ;
#19440 = DIRECTION ( 'NONE',  ( 1.000000000000000000, 0.000000000000000000, 0.000000000000000000 ) ) ;
#19441 = ORIENTED_EDGE ( 'NONE', *, *, #1832, .T. ) ;
#19442 = ORIENTED_EDGE ( 'NONE', *, *, #21439, .T. ) ;
#19443 = CARTESIAN_POINT ( 'NONE',  ( 1.724728116533979838, 42.36054587065083155, 41.66679706732590915 ) ) ;
#19444 = CARTESIAN_POINT ( 'NONE',  ( -27.37540678000428684, -36.74634676501047181, 42.50000000000000000 ) ) ;
#19445 = EDGE_CURVE ( 'NONE', #17182, #299, #4838, .T. ) ;
#19446 = CYLINDRICAL_SURFACE ( 'NONE', #20721, 0.2499999999999985845 ) ;
#19447 = CIRCLE ( 'NONE', #16573, 1.000000000000000000 ) ;
#19448 = CARTESIAN_POINT ( 'NONE',  ( 15.21174975910707161, 32.10873716947361345, 68.25000000000000000 ) ) ;
#19449 = LINE ( 'NONE', #19909, #8175 ) ;
#19450 = DIRECTION ( 'NONE',  ( 0.000000000000000000, -0.000000000000000000, 1.000000000000000000 ) ) ;
#19451 = ORIENTED_EDGE ( 'NONE', *, *, #16182, .F. ) ;
#19452 = CARTESIAN_POINT ( 'NONE',  ( -9.178906393579158163, 42.46645089659918426, 68.06527860057354928 ) ) ;
#19453 = ADVANCED_FACE ( 'NONE', ( #15121 ), #21968, .T. ) ;
#19454 = LINE ( 'NONE', #21258, #21430 ) ;
#19455 = DIRECTION ( 'NONE',  ( -1.000000000000000000, 0.000000000000000000, 0.000000000000000000 ) ) ;
#19456 = EDGE_LOOP ( 'NONE', ( #20414, #1403, #7651, #2956 ) ) ;
#19457 = DIRECTION ( 'NONE',  ( -4.336808689941893885E-15, 0.000000000000000000, 1.000000000000000000 ) ) ;
#19458 = ORIENTED_EDGE ( 'NONE', *, *, #15780, .F. ) ;
#19459 = ORIENTED_EDGE ( 'NONE', *, *, #371, .F. ) ;
#19460 = AXIS2_PLACEMENT_3D ( 'NONE', #14098, #20949, #14224 ) ;
#19461 = VERTEX_POINT ( 'NONE', #2139 ) ;
#19462 = CARTESIAN_POINT ( 'NONE',  ( 27.37540678000427619, 10.94079601157914539, 42.50000000000000000 ) ) ;
#19463 = ORIENTED_EDGE ( 'NONE', *, *, #8826, .T. ) ;
#19464 = ORIENTED_EDGE ( 'NONE', *, *, #4413, .F. ) ;
#19465 = EDGE_CURVE ( 'NONE', #823, #1780, #4916, .T. ) ;
#19466 = CARTESIAN_POINT ( 'NONE',  ( 3.627054932750481964, 32.11873716947361856, 68.00000000000000000 ) ) ;
#19467 = VERTEX_POINT ( 'NONE', #14215 ) ;
#19468 = DIRECTION ( 'NONE',  ( -0.000000000000000000, 0.000000000000000000, 1.000000000000000000 ) ) ;
#19469 = DIRECTION ( 'NONE',  ( -1.000000000000000000, 0.000000000000000000, 0.000000000000000000 ) ) ;
#19470 = LINE ( 'NONE', #7632, #11649 ) ;
#19471 = CARTESIAN_POINT ( 'NONE',  ( -1.824728116533986810, 43.31054587065082728, 35.70876104995653577 ) ) ;
#19472 = AXIS2_PLACEMENT_3D ( 'NONE', #16455, #18578, #2817 ) ;
#19473 =( GEOMETRIC_REPRESENTATION_CONTEXT ( 3 ) GLOBAL_UNCERTAINTY_ASSIGNED_CONTEXT ( ( #21634 ) ) GLOBAL_UNIT_ASSIGNED_CONTEXT ( ( #17635, #17203, #4009 ) ) REPRESENTATION_CONTEXT ( 'NONE', 'WORKASPACE' ) );
#19474 = LINE ( 'NONE', #17351, #5393 ) ;
#19475 = EDGE_CURVE ( 'NONE', #20345, #19696, #17404, .T. ) ;
#19476 = EDGE_CURVE ( 'NONE', #17830, #6583, #15608, .T. ) ;
#19477 = FACE_OUTER_BOUND ( 'NONE', #17542, .T. ) ;
#19478 = ADVANCED_FACE ( 'NONE', ( #13885 ), #19049, .T. ) ;
#19479 = DIRECTION ( 'NONE',  ( 1.000000000000000000, -0.000000000000000000, 6.123233995736764803E-17 ) ) ;
#19480 = DIRECTION ( 'NONE',  ( -0.000000000000000000, 0.000000000000000000, -1.000000000000000000 ) ) ;
#19481 = CARTESIAN_POINT ( 'NONE',  ( 1.724728116533979616, 42.36054587065083155, 47.75876104995653293 ) ) ;
#19482 = ADVANCED_FACE ( 'NONE', ( #8753 ), #12096, .T. ) ;
#19483 = CARTESIAN_POINT ( 'NONE',  ( -32.29156311937309454, 83.96304096052088539, 13.75000000000000000 ) ) ;
#19484 = ORIENTED_EDGE ( 'NONE', *, *, #2794, .F. ) ;
#19485 = VECTOR ( 'NONE', #5284, 1000.000000000000000 ) ;
#19486 = ORIENTED_EDGE ( 'NONE', *, *, #14541, .F. ) ;
#19487 = DIRECTION ( 'NONE',  ( 0.000000000000000000, 1.000000000000000000, 0.000000000000000000 ) ) ;
#19488 = AXIS2_PLACEMENT_3D ( 'NONE', #10570, #11111, #21546 ) ;
#19489 = AXIS2_PLACEMENT_3D ( 'NONE', #20976, #7007, #7330 ) ;
#19490 = VECTOR ( 'NONE', #12802, 1000.000000000000000 ) ;
#19491 = ORIENTED_EDGE ( 'NONE', *, *, #16489, .T. ) ;
#19492 = EDGE_CURVE ( 'NONE', #15133, #6809, #16683, .T. ) ;
#19493 = DIRECTION ( 'NONE',  ( -0.000000000000000000, -1.000000000000000000, -0.000000000000000000 ) ) ;
#19494 = VECTOR ( 'NONE', #44, 1000.000000000000000 ) ;
#19495 = DIRECTION ( 'NONE',  ( -1.000000000000000000, 0.000000000000000000, 0.000000000000000000 ) ) ;
#19496 = AXIS2_PLACEMENT_3D ( 'NONE', #1815, #7408, #17244 ) ;
#19497 = ORIENTED_EDGE ( 'NONE', *, *, #14677, .T. ) ;
#19498 = CARTESIAN_POINT ( 'NONE',  ( -32.23382792203229741, 83.71979900898287497, 68.25000000000000000 ) ) ;
#19499 = DIRECTION ( 'NONE',  ( -0.000000000000000000, -0.000000000000000000, -1.000000000000000000 ) ) ;
#19500 = ADVANCED_FACE ( 'NONE', ( #229 ), #15880, .F. ) ;
#19501 = CARTESIAN_POINT ( 'NONE',  ( 1.724728116533979616, 43.26054587065083012, 39.70876104995653577 ) ) ;
#19502 = DIRECTION ( 'NONE',  ( -0.000000000000000000, 0.000000000000000000, -1.000000000000000000 ) ) ;
#19503 = CARTESIAN_POINT ( 'NONE',  ( -23.14079623692856913, 2.756488901337824426, 13.42422799743261308 ) ) ;
#19504 = AXIS2_PLACEMENT_3D ( 'NONE', #2806, #11081, #16103 ) ;
#19505 = AXIS2_PLACEMENT_3D ( 'NONE', #5329, #5203, #21993 ) ;
#19506 = ADVANCED_FACE ( 'NONE', ( #19377 ), #10651, .F. ) ;
#19507 = ORIENTED_EDGE ( 'NONE', *, *, #8347, .T. ) ;
#19508 = CARTESIAN_POINT ( 'NONE',  ( 29.13662752439705272, -5.000000000000000000, 3.799999999999999822 ) ) ;
#19509 = DIRECTION ( 'NONE',  ( 0.000000000000000000, 0.000000000000000000, -1.000000000000000000 ) ) ;
#19510 = DIRECTION ( 'NONE',  ( 0.000000000000000000, 1.000000000000000000, 0.000000000000000000 ) ) ;
#19511 = EDGE_LOOP ( 'NONE', ( #14589, #16499, #7245, #5994 ) ) ;
#19512 = VERTEX_POINT ( 'NONE', #1912 ) ;
#19513 = VERTEX_POINT ( 'NONE', #5408 ) ;
#19514 = CARTESIAN_POINT ( 'NONE',  ( -1.724728116533986721, 43.26054587065083012, 43.70876104995653577 ) ) ;
#19515 = CARTESIAN_POINT ( 'NONE',  ( 25.37540678000427263, -63.74634676501045050, 3.799999999999999822 ) ) ;
#19516 = ORIENTED_EDGE ( 'NONE', *, *, #17564, .F. ) ;
#19517 = TOROIDAL_SURFACE ( 'NONE', #2362, 2.076718556943726313, 0.2500000000000000000 ) ;
#19518 = AXIS2_PLACEMENT_3D ( 'NONE', #19010, #15949, #17307 ) ;
#19519 = DIRECTION ( 'NONE',  ( 0.000000000000000000, 0.000000000000000000, 1.000000000000000000 ) ) ;
#19520 = AXIS2_PLACEMENT_3D ( 'NONE', #10053, #16525, #6259 ) ;
#19521 = ORIENTED_EDGE ( 'NONE', *, *, #14958, .T. ) ;
#19522 = FACE_OUTER_BOUND ( 'NONE', #6031, .T. ) ;
#19523 = AXIS2_PLACEMENT_3D ( 'NONE', #12881, #9545, #4395 ) ;
#19524 = DIRECTION ( 'NONE',  ( 1.000000000000000000, 0.000000000000000000, 0.000000000000000000 ) ) ;
#19525 = EDGE_CURVE ( 'NONE', #12110, #538, #17245, .T. ) ;
#19526 = CARTESIAN_POINT ( 'NONE',  ( 15.21174975910705918, -51.61873716947361856, 14.00000000000000000 ) ) ;
#19527 = DIRECTION ( 'NONE',  ( -1.000000000000000000, 0.000000000000000000, 0.000000000000000000 ) ) ;
#19528 = DIRECTION ( 'NONE',  ( 0.000000000000000000, 1.000000000000000000, 0.000000000000000000 ) ) ;
#19529 = CARTESIAN_POINT ( 'NONE',  ( -31.26086011588027347, 83.95073979834609190, 13.75000000000000000 ) ) ;
#19530 = ORIENTED_EDGE ( 'NONE', *, *, #11469, .T. ) ;
#19531 = DIRECTION ( 'NONE',  ( -1.224646799147353207E-16, -0.000000000000000000, -1.000000000000000000 ) ) ;
#19532 = CARTESIAN_POINT ( 'NONE',  ( 1.724728116533979616, 43.26054587065083012, 39.80876104995653719 ) ) ;
#19533 = PLANE ( 'NONE',  #4075 ) ;
#19534 = CARTESIAN_POINT ( 'NONE',  ( -23.32398829872514057, -3.528912754968629439, 13.50000000000000000 ) ) ;
#19535 = ORIENTED_EDGE ( 'NONE', *, *, #2240, .T. ) ;
#19536 = VECTOR ( 'NONE', #21780, 1000.000000000000000 ) ;
#19537 = CIRCLE ( 'NONE', #3815, 0.05000000000000143219 ) ;
#19538 = CIRCLE ( 'NONE', #13823, 0.2999999999999999334 ) ;
#19539 = CARTESIAN_POINT ( 'NONE',  ( -15.95292532278785913, -52.10286008774954780, 13.87500000000000000 ) ) ;
#19540 = ADVANCED_FACE ( 'NONE', ( #3612 ), #12528, .T. ) ;
#19541 = AXIS2_PLACEMENT_3D ( 'NONE', #6600, #1770, #1309 ) ;
#19542 = ORIENTED_EDGE ( 'NONE', *, *, #12099, .F. ) ;
#19543 = CARTESIAN_POINT ( 'NONE',  ( 18.22752199202934520, 50.11873716947361856, 13.79999999999999893 ) ) ;
#19544 = CARTESIAN_POINT ( 'NONE',  ( 14.71174975910705740, 50.19799549595485644, 13.75000000000000000 ) ) ;
#19545 = ORIENTED_EDGE ( 'NONE', *, *, #17580, .T. ) ;
#19546 = CIRCLE ( 'NONE', #9902, 0.2999999999999999334 ) ;
#19547 = VERTEX_POINT ( 'NONE', #10436 ) ;
#19548 = CARTESIAN_POINT ( 'NONE',  ( -14.96502315657345328, 51.87273146205216534, 13.83570993898299406 ) ) ;
#19549 = DIRECTION ( 'NONE',  ( 0.000000000000000000, 0.000000000000000000, -1.000000000000000000 ) ) ;
#19550 = LINE ( 'NONE', #6143, #5687 ) ;
#19551 = ORIENTED_EDGE ( 'NONE', *, *, #10892, .F. ) ;
#19552 = AXIS2_PLACEMENT_3D ( 'NONE', #5518, #347, #5749 ) ;
#19553 = ORIENTED_EDGE ( 'NONE', *, *, #5906, .T. ) ;
#19554 = CIRCLE ( 'NONE', #9912, 0.2999999999999999334 ) ;
#19555 = AXIS2_PLACEMENT_3D ( 'NONE', #537, #10846, #662 ) ;
#19556 = EDGE_CURVE ( 'NONE', #21336, #21055, #18941, .T. ) ;
#19557 = ORIENTED_EDGE ( 'NONE', *, *, #17137, .T. ) ;
#19558 = CARTESIAN_POINT ( 'NONE',  ( 0.000000000000000000, 42.31054587065082728, 51.75876104995654003 ) ) ;
#19559 = CIRCLE ( 'NONE', #6001, 0.2500000000000002220 ) ;
#19560 = EDGE_CURVE ( 'NONE', #20727, #19811, #12706, .T. ) ;
#19561 = DIRECTION ( 'NONE',  ( -1.000000000000000000, 0.000000000000000000, -0.000000000000000000 ) ) ;
#19562 = DIRECTION ( 'NONE',  ( -1.000000000000000000, 0.000000000000000000, 0.000000000000000000 ) ) ;
#19563 = CARTESIAN_POINT ( 'NONE',  ( -28.57540678000427548, 0.000000000000000000, 13.19999999999999929 ) ) ;
#19564 = DIRECTION ( 'NONE',  ( 0.000000000000000000, -0.000000000000000000, -1.000000000000000000 ) ) ;
#19565 = FACE_OUTER_BOUND ( 'NONE', #9031, .T. ) ;
#19566 = ORIENTED_EDGE ( 'NONE', *, *, #6884, .T. ) ;
#19567 = DIRECTION ( 'NONE',  ( 0.000000000000000000, 0.000000000000000000, 1.000000000000000000 ) ) ;
#19568 = DIRECTION ( 'NONE',  ( 0.000000000000000000, 0.000000000000000000, -1.000000000000000000 ) ) ;
#19569 = DIRECTION ( 'NONE',  ( -1.000000000000000000, 0.000000000000000000, -0.000000000000000000 ) ) ;
#19570 = AXIS2_PLACEMENT_3D ( 'NONE', #21481, #18086, #1417 ) ;
#19571 = VECTOR ( 'NONE', #12499, 1000.000000000000114 ) ;
#19572 = CIRCLE ( 'NONE', #22100, 3.500000000000003109 ) ;
#19573 = CARTESIAN_POINT ( 'NONE',  ( 1.724728116533979838, 43.26054587065083012, 53.71679706732590631 ) ) ;
#19574 = ORIENTED_EDGE ( 'NONE', *, *, #4968, .T. ) ;
#19575 = CIRCLE ( 'NONE', #8868, 0.5000000000000004441 ) ;
#19576 = EDGE_CURVE ( 'NONE', #14923, #22131, #5249, .T. ) ;
#19577 = EDGE_LOOP ( 'NONE', ( #16596, #12435, #19438, #10050 ) ) ;
#19578 = VECTOR ( 'NONE', #13220, 1000.000000000000000 ) ;
#19579 = ORIENTED_EDGE ( 'NONE', *, *, #16305, .T. ) ;
#19580 = CARTESIAN_POINT ( 'NONE',  ( -17.95292532278785913, 50.11873716947361856, 68.00000000000000000 ) ) ;
#19581 = AXIS2_PLACEMENT_3D ( 'NONE', #2933, #6420, #9760 ) ;
#19582 = APPLICATION_PROTOCOL_DEFINITION ( 'draft international standard', 'automotive_design', 1998, #3150 ) ;
#19583 = ORIENTED_EDGE ( 'NONE', *, *, #13225, .T. ) ;
#19584 = EDGE_LOOP ( 'NONE', ( #13564, #17276, #12908, #16093, #14762, #17541, #9981, #21784 ) ) ;
#19585 = EDGE_CURVE ( 'NONE', #833, #11510, #14863, .T. ) ;
#19586 = EDGE_CURVE ( 'NONE', #13584, #14169, #5960, .T. ) ;
#19587 = CARTESIAN_POINT ( 'NONE',  ( 3.127054932750481964, 33.43424481021354921, 68.00000000000000000 ) ) ;
#19588 = VERTEX_POINT ( 'NONE', #20944 ) ;
#19589 = DIRECTION ( 'NONE',  ( 0.000000000000000000, 0.000000000000000000, -1.000000000000000000 ) ) ;
#19590 = TOROIDAL_SURFACE ( 'NONE', #18509, 0.2500000000000000000, 0.2500000000000000000 ) ;
#19591 = TOROIDAL_SURFACE ( 'NONE', #14211, 0.05000000000000000278, 0.05000000000000000278 ) ;
#19592 = ORIENTED_EDGE ( 'NONE', *, *, #12686, .T. ) ;
#19593 = CARTESIAN_POINT ( 'NONE',  ( 1.724728116533979838, 43.31054587065082728, 45.66679706732590205 ) ) ;
#19594 = CARTESIAN_POINT ( 'NONE',  ( 32.20000000000001705, 72.00000000000001421, 1.800000000000000044 ) ) ;
#19595 = VECTOR ( 'NONE', #9944, 1000.000000000000000 ) ;
#19596 = AXIS2_PLACEMENT_3D ( 'NONE', #13977, #17335, #12185 ) ;
#19597 = CARTESIAN_POINT ( 'NONE',  ( -9.141460742840918030, -33.43424481021354921, 7.321391277662001151 ) ) ;
#19598 = CIRCLE ( 'NONE', #10655, 0.3000000000000016542 ) ;
#19599 = LINE ( 'NONE', #16453, #16932 ) ;
#19600 = CARTESIAN_POINT ( 'NONE',  ( 25.37540678000426908, 36.74634676501047181, 13.79999999999999893 ) ) ;
#19601 = DIRECTION ( 'NONE',  ( 0.000000000000000000, 0.000000000000000000, -1.000000000000000000 ) ) ;
#19602 = LINE ( 'NONE', #6078, #5404 ) ;
#19603 = EDGE_CURVE ( 'NONE', #21679, #12877, #5629, .T. ) ;
#19604 = LINE ( 'NONE', #4384, #20615 ) ;
#19605 = AXIS2_PLACEMENT_3D ( 'NONE', #980, #12098, #5304 ) ;
#19606 = CARTESIAN_POINT ( 'NONE',  ( -8.638906393579159015, 43.42161583426526761, 69.94509975324525897 ) ) ;
#19607 = ORIENTED_EDGE ( 'NONE', *, *, #8396, .F. ) ;
#19608 = ORIENTED_EDGE ( 'NONE', *, *, #12144, .F. ) ;
#19609 = DIRECTION ( 'NONE',  ( -0.000000000000000000, -1.000000000000000000, -0.000000000000000000 ) ) ;
#19610 = ORIENTED_EDGE ( 'NONE', *, *, #1967, .T. ) ;
#19611 = AXIS2_PLACEMENT_3D ( 'NONE', #9384, #21252, #17877 ) ;
#19612 = EDGE_LOOP ( 'NONE', ( #14569, #17111, #6799, #4700 ) ) ;
#19613 = EDGE_CURVE ( 'NONE', #20955, #20601, #11293, .T. ) ;
#19614 = ADVANCED_FACE ( 'NONE', ( #21512 ), #19517, .T. ) ;
#19615 = EDGE_CURVE ( 'NONE', #689, #16405, #4158, .T. ) ;
#19616 = DIRECTION ( 'NONE',  ( -0.000000000000000000, -0.000000000000000000, -1.000000000000000000 ) ) ;
#19617 = DIRECTION ( 'NONE',  ( -1.000000000000000000, 0.000000000000000000, 0.000000000000000000 ) ) ;
#19618 = ORIENTED_EDGE ( 'NONE', *, *, #8634, .F. ) ;
#19619 = SURFACE_STYLE_USAGE ( .BOTH. , #5981 ) ;
#19620 = CARTESIAN_POINT ( 'NONE',  ( -23.83662752439705201, 0.000000000000000000, 7.500000000000000000 ) ) ;
#19621 = CIRCLE ( 'NONE', #21065, 0.1000000000000028644 ) ;
#19622 = DIRECTION ( 'NONE',  ( 0.000000000000000000, 0.000000000000000000, 1.000000000000000000 ) ) ;
#19623 = DIRECTION ( 'NONE',  ( 0.000000000000000000, 0.000000000000000000, 1.000000000000000000 ) ) ;
#19624 = LINE ( 'NONE', #12557, #3416 ) ;
#19625 = AXIS2_PLACEMENT_3D ( 'NONE', #10628, #15860, #10843 ) ;
#19626 = EDGE_CURVE ( 'NONE', #12853, #13036, #2684, .T. ) ;
#19627 = ORIENTED_EDGE ( 'NONE', *, *, #3687, .F. ) ;
#19628 = CARTESIAN_POINT ( 'NONE',  ( 17.95292532278785913, 38.74634676501045760, 109.6002446535588319 ) ) ;
#19629 = CARTESIAN_POINT ( 'NONE',  ( -7.347880794884131322E-17, -85.00000000000000000, 1.200000000000002176 ) ) ;
#19630 = DIRECTION ( 'NONE',  ( -1.000000000000000000, 0.000000000000000000, 0.000000000000000000 ) ) ;
#19631 = ORIENTED_EDGE ( 'NONE', *, *, #11637, .F. ) ;
#19632 = EDGE_LOOP ( 'NONE', ( #21741, #2989, #11372, #14207 ) ) ;
#19633 = EDGE_LOOP ( 'NONE', ( #16535, #7213, #6138, #12249 ) ) ;
#19634 = DIRECTION ( 'NONE',  ( 0.000000000000000000, -0.000000000000000000, 1.000000000000000000 ) ) ;
#19635 = CARTESIAN_POINT ( 'NONE',  ( 29.37540678000427619, -4.700000000000000178, 3.500000000000000000 ) ) ;
#19636 = ORIENTED_EDGE ( 'NONE', *, *, #18469, .F. ) ;
#19637 = PLANE ( 'NONE',  #17357 ) ;
#19638 = EDGE_CURVE ( 'NONE', #16219, #9468, #10234, .T. ) ;
#19639 = CIRCLE ( 'NONE', #9652, 0.2999999999999999334 ) ;
#19640 = AXIS2_PLACEMENT_3D ( 'NONE', #10217, #20517, #17033 ) ;
#19641 = AXIS2_PLACEMENT_3D ( 'NONE', #16780, #3140, #15202 ) ;
#19642 = EDGE_CURVE ( 'NONE', #4505, #21013, #15572, .T. ) ;
#19643 = ORIENTED_EDGE ( 'NONE', *, *, #2298, .F. ) ;
#19644 = DIRECTION ( 'NONE',  ( 0.000000000000000000, 0.000000000000000000, 1.000000000000000000 ) ) ;
#19645 = LINE ( 'NONE', #12465, #15943 ) ;
#19646 = EDGE_CURVE ( 'NONE', #20083, #14314, #17007, .T. ) ;
#19647 = DIRECTION ( 'NONE',  ( 0.000000000000000000, 0.000000000000000000, -1.000000000000000000 ) ) ;
#19648 = CYLINDRICAL_SURFACE ( 'NONE', #8799, 0.04999999999999991257 ) ;
#19649 = DIRECTION ( 'NONE',  ( -1.000000000000000000, 0.000000000000000000, 0.000000000000000000 ) ) ;
#19650 = LINE ( 'NONE', #6125, #4852 ) ;
#19651 = ORIENTED_EDGE ( 'NONE', *, *, #17737, .T. ) ;
#19652 = CARTESIAN_POINT ( 'NONE',  ( -14.96174975910705207, 41.81054587065082728, 13.75000000000000000 ) ) ;
#19653 = DIRECTION ( 'NONE',  ( -1.000000000000000000, -0.000000000000000000, -4.336808689942194441E-15 ) ) ;
#19654 = CARTESIAN_POINT ( 'NONE',  ( -15.95292532278785913, -50.11873716947361856, 13.99999999999999822 ) ) ;
#19655 = DIRECTION ( 'NONE',  ( -0.000000000000000000, -0.000000000000000000, 1.000000000000000000 ) ) ;
#19656 = ORIENTED_EDGE ( 'NONE', *, *, #9904, .T. ) ;
#19657 = DIRECTION ( 'NONE',  ( 0.000000000000000000, 0.000000000000000000, 1.000000000000000000 ) ) ;
#19658 = AXIS2_PLACEMENT_3D ( 'NONE', #2518, #8120, #938 ) ;
#19659 = ADVANCED_FACE ( 'NONE', ( #4601 ), #14425, .F. ) ;
#19660 = VERTEX_POINT ( 'NONE', #11415 ) ;
#19661 = AXIS2_PLACEMENT_3D ( 'NONE', #16968, #8482, #9825 ) ;
#19662 = TOROIDAL_SURFACE ( 'NONE', #21112, 0.05000000000000000278, 0.05000000000000000278 ) ;
#19663 = FACE_OUTER_BOUND ( 'NONE', #21022, .T. ) ;
#19664 = LINE ( 'NONE', #21470, #8115 ) ;
#19665 = VERTEX_POINT ( 'NONE', #4151 ) ;
#19666 = ORIENTED_EDGE ( 'NONE', *, *, #731, .T. ) ;
#19667 = PLANE ( 'NONE',  #10620 ) ;
#19668 = DIRECTION ( 'NONE',  ( 0.000000000000000000, 0.000000000000000000, -1.000000000000000000 ) ) ;
#19669 = ADVANCED_FACE ( 'NONE', ( #7528 ), #14488, .T. ) ;
#19670 = DIRECTION ( 'NONE',  ( 1.000000000000000000, -1.094601647044990554E-16, -0.000000000000000000 ) ) ;
#19671 = EDGE_LOOP ( 'NONE', ( #7103, #11181, #9279, #12020, #4908, #3544 ) ) ;
#19672 = VERTEX_POINT ( 'NONE', #6073 ) ;
#19673 = DIRECTION ( 'NONE',  ( -0.000000000000000000, -0.000000000000000000, -1.000000000000000000 ) ) ;
#19674 = EDGE_CURVE ( 'NONE', #9132, #1830, #4862, .T. ) ;
#19675 = CIRCLE ( 'NONE', #4306, 0.1000000000000028644 ) ;
#19676 = CARTESIAN_POINT ( 'NONE',  ( 17.95292532278785913, 50.11873716947361856, 14.00000000000000000 ) ) ;
#19677 = DIRECTION ( 'NONE',  ( 0.000000000000000000, 1.000000000000000000, 0.000000000000000000 ) ) ;
#19678 = AXIS2_PLACEMENT_3D ( 'NONE', #12968, #16213, #11417 ) ;
#19679 = FACE_OUTER_BOUND ( 'NONE', #17958, .T. ) ;
#19680 = LINE ( 'NONE', #4351, #16126 ) ;
#19681 = CARTESIAN_POINT ( 'NONE',  ( -23.13310673709249343, 45.37789868843801599, 13.50000000000000000 ) ) ;
#19682 = DIRECTION ( 'NONE',  ( 1.000000000000000000, -0.000000000000000000, -0.000000000000000000 ) ) ;
#19683 = LINE ( 'NONE', #3716, #652 ) ;
#19684 = ORIENTED_EDGE ( 'NONE', *, *, #11172, .F. ) ;
#19685 = CARTESIAN_POINT ( 'NONE',  ( -24.94594744299175915, 42.46645089659918426, 68.50000000000000000 ) ) ;
#19686 = DIRECTION ( 'NONE',  ( 0.2309407893632116904, -0.9729678061520312671, 0.000000000000000000 ) ) ;
#19687 = DIRECTION ( 'NONE',  ( -0.000000000000000000, 0.000000000000000000, 1.000000000000000000 ) ) ;
#19688 = EDGE_CURVE ( 'NONE', #8431, #9468, #14535, .T. ) ;
#19689 = CARTESIAN_POINT ( 'NONE',  ( -28.87540678000427619, 63.74634676501045050, 13.19999999999999929 ) ) ;
#19690 = ORIENTED_EDGE ( 'NONE', *, *, #21321, .T. ) ;
#19691 = EDGE_CURVE ( 'NONE', #20699, #12236, #16649, .T. ) ;
#19692 = ADVANCED_FACE ( 'NONE', ( #12858 ), #909, .T. ) ;
#19693 = ORIENTED_EDGE ( 'NONE', *, *, #7319, .F. ) ;
#19694 = DIRECTION ( 'NONE',  ( 1.000000000000000000, 0.000000000000000000, 0.000000000000000000 ) ) ;
#19695 = EDGE_LOOP ( 'NONE', ( #11098, #21548, #8249, #15082 ) ) ;
#19696 = VERTEX_POINT ( 'NONE', #11083 ) ;
#19697 = DIRECTION ( 'NONE',  ( 0.000000000000000000, -1.000000000000000000, 0.000000000000000000 ) ) ;
#19698 = CARTESIAN_POINT ( 'NONE',  ( -15.95292532278785913, -52.39333383871510108, 13.50000000000000000 ) ) ;
#19699 = ORIENTED_EDGE ( 'NONE', *, *, #16966, .T. ) ;
#19700 = DIRECTION ( 'NONE',  ( 0.000000000000000000, 0.000000000000000000, -1.000000000000000000 ) ) ;
#19701 = AXIS2_PLACEMENT_3D ( 'NONE', #2390, #9223, #9108 ) ;
#19702 = ORIENTED_EDGE ( 'NONE', *, *, #1733, .F. ) ;
#19703 = CARTESIAN_POINT ( 'NONE',  ( 15.21174975910705918, 41.81054587065082728, 13.50000000000000000 ) ) ;
#19704 = DIRECTION ( 'NONE',  ( 1.000000000000000000, 0.000000000000000000, 0.000000000000000000 ) ) ;
#19705 = DIRECTION ( 'NONE',  ( 0.000000000000000000, -0.000000000000000000, -1.000000000000000000 ) ) ;
#19706 = CIRCLE ( 'NONE', #2193, 6.499999999999999112 ) ;
#19707 = EDGE_CURVE ( 'NONE', #8649, #6333, #3796, .T. ) ;
#19708 = PLANE ( 'NONE',  #16452 ) ;
#19709 = DIRECTION ( 'NONE',  ( -1.000000000000000000, -0.000000000000000000, -0.000000000000000000 ) ) ;
#19710 = VECTOR ( 'NONE', #21204, 1000.000000000000000 ) ;
#19711 = DIRECTION ( 'NONE',  ( -0.000000000000000000, 0.000000000000000000, -1.000000000000000000 ) ) ;
#19712 = FACE_OUTER_BOUND ( 'NONE', #5360, .T. ) ;
#19713 = CARTESIAN_POINT ( 'NONE',  ( -28.87540678000427619, -6.494748934539263274, 7.799999999999999822 ) ) ;
#19714 = CIRCLE ( 'NONE', #2204, 0.05000000000000143219 ) ;
#19715 = ADVANCED_FACE ( 'NONE', ( #11187 ), #7737, .T. ) ;
#19716 = CIRCLE ( 'NONE', #6879, 1.000000000000000888 ) ;
#19717 = ORIENTED_EDGE ( 'NONE', *, *, #7199, .F. ) ;
#19718 = DIRECTION ( 'NONE',  ( 1.000000000000000000, 0.000000000000000000, 0.000000000000000000 ) ) ;
#19719 = VECTOR ( 'NONE', #18793, 1000.000000000000000 ) ;
#19720 = CARTESIAN_POINT ( 'NONE',  ( 27.37540678000427974, -10.94079601157914716, 42.50000000000000000 ) ) ;
#19721 = ORIENTED_EDGE ( 'NONE', *, *, #20411, .F. ) ;
#19722 = ORIENTED_EDGE ( 'NONE', *, *, #7782, .F. ) ;
#19723 = DIRECTION ( 'NONE',  ( -1.000000000000000000, -5.192538640813645496E-17, 7.145994714117440585E-17 ) ) ;
#19724 = VERTEX_POINT ( 'NONE', #7859 ) ;
#19725 = SURFACE_SIDE_STYLE ('',( #6540 ) ) ;
#19726 = ORIENTED_EDGE ( 'NONE', *, *, #12644, .T. ) ;
#19727 = AXIS2_PLACEMENT_3D ( 'NONE', #725, #7578, #14710 ) ;
#19728 = ORIENTED_EDGE ( 'NONE', *, *, #7666, .T. ) ;
#19729 = VECTOR ( 'NONE', #4272, 1000.000000000000000 ) ;
#19730 = DIRECTION ( 'NONE',  ( 1.000000000000000000, 0.000000000000000000, -0.000000000000000000 ) ) ;
#19731 = VECTOR ( 'NONE', #2777, 1000.000000000000000 ) ;
#19732 = CARTESIAN_POINT ( 'NONE',  ( -26.37540678000427619, -10.94079601157914716, 42.50000000000000000 ) ) ;
#19733 = VERTEX_POINT ( 'NONE', #14654 ) ;
#19734 = DIRECTION ( 'NONE',  ( -0.000000000000000000, -0.000000000000000000, 1.000000000000000000 ) ) ;
#19735 = CARTESIAN_POINT ( 'NONE',  ( 14.66174954729678248, 51.84624528035402591, 13.50000000000000000 ) ) ;
#19736 = CYLINDRICAL_SURFACE ( 'NONE', #1125, 2.000000000000001776 ) ;
#19737 = CARTESIAN_POINT ( 'NONE',  ( -23.02398829872514341, 2.280095008958276104, 13.43080372783514598 ) ) ;
#19738 = EDGE_CURVE ( 'NONE', #9842, #8846, #21618, .T. ) ;
#19739 = ORIENTED_EDGE ( 'NONE', *, *, #8910, .T. ) ;
#19740 = DIRECTION ( 'NONE',  ( 0.000000000000000000, 0.000000000000000000, 1.000000000000000000 ) ) ;
#19741 = DIRECTION ( 'NONE',  ( -1.000000000000000000, 0.000000000000000000, 0.000000000000000000 ) ) ;
#19742 = ADVANCED_FACE ( 'NONE', ( #22154 ), #15507, .T. ) ;
#19743 = ORIENTED_EDGE ( 'NONE', *, *, #6784, .F. ) ;
#19744 = ORIENTED_EDGE ( 'NONE', *, *, #15483, .T. ) ;
#19745 = ORIENTED_EDGE ( 'NONE', *, *, #17254, .T. ) ;
#19746 = CYLINDRICAL_SURFACE ( 'NONE', #3500, 0.3000000000000016542 ) ;
#19747 = AXIS2_PLACEMENT_3D ( 'NONE', #9734, #19569, #9283 ) ;
#19748 = DIRECTION ( 'NONE',  ( -0.8949343913984425525, -2.944963428651749748E-15, 0.4461977533474358326 ) ) ;
#19749 = VERTEX_POINT ( 'NONE', #6933 ) ;
#19750 = AXIS2_PLACEMENT_3D ( 'NONE', #17965, #8016, #4541 ) ;
#19751 = CARTESIAN_POINT ( 'NONE',  ( -32.48382792203229741, 83.71979900898287497, 68.50000000000000000 ) ) ;
#19752 = ADVANCED_FACE ( 'NONE', ( #7146 ), #13622, .F. ) ;
#19753 = VERTEX_POINT ( 'NONE', #3335 ) ;
#19754 = DIRECTION ( 'NONE',  ( 0.000000000000000000, 0.000000000000000000, 1.000000000000000000 ) ) ;
#19755 = CARTESIAN_POINT ( 'NONE',  ( -1.824728116533986810, 43.26054587065083012, 33.66679706732590915 ) ) ;
#19756 = TOROIDAL_SURFACE ( 'NONE', #10463, 2.274596669241483848, 0.2999999999999999889 ) ;
#19757 = EDGE_CURVE ( 'NONE', #16569, #1455, #10938, .T. ) ;
#19758 = DIRECTION ( 'NONE',  ( 0.000000000000000000, 0.000000000000000000, -1.000000000000000000 ) ) ;
#19759 = CARTESIAN_POINT ( 'NONE',  ( -29.69597781366221412, 26.24124249474150972, 68.75000000000000000 ) ) ;
#19760 = CARTESIAN_POINT ( 'NONE',  ( 15.21174975910705918, 51.61873716947361856, 14.00000000000000000 ) ) ;
#19761 = FACE_OUTER_BOUND ( 'NONE', #13189, .T. ) ;
#19762 = ORIENTED_EDGE ( 'NONE', *, *, #1768, .T. ) ;
#19763 = DIRECTION ( 'NONE',  ( -0.000000000000000000, -1.000000000000000000, -0.000000000000000000 ) ) ;
#19764 = DIRECTION ( 'NONE',  ( -0.000000000000000000, 1.000000000000000000, -0.000000000000000000 ) ) ;
#19765 = FACE_OUTER_BOUND ( 'NONE', #10833, .T. ) ;
#19766 = DIRECTION ( 'NONE',  ( 0.000000000000000000, 0.000000000000000000, 1.000000000000000000 ) ) ;
#19767 = ORIENTED_EDGE ( 'NONE', *, *, #15757, .T. ) ;
#19768 = DIRECTION ( 'NONE',  ( 0.000000000000000000, 0.000000000000000000, 1.000000000000000000 ) ) ;
#19769 = LINE ( 'NONE', #18195, #16089 ) ;
#19770 = ADVANCED_FACE ( 'NONE', ( #5020 ), #1640, .F. ) ;
#19771 = ADVANCED_FACE ( 'NONE', ( #11931 ), #12259, .F. ) ;
#19772 = ORIENTED_EDGE ( 'NONE', *, *, #19613, .F. ) ;
#19773 = DIRECTION ( 'NONE',  ( -0.000000000000000000, 1.000000000000000000, -0.000000000000000000 ) ) ;
#19774 = ADVANCED_FACE ( 'NONE', ( #19000 ), #17197, .T. ) ;
#19775 = LINE ( 'NONE', #2882, #3087 ) ;
#19776 = ORIENTED_EDGE ( 'NONE', *, *, #6612, .F. ) ;
#19777 = VERTEX_POINT ( 'NONE', #15938 ) ;
#19778 = DIRECTION ( 'NONE',  ( -0.000000000000000000, -0.000000000000000000, -1.000000000000000000 ) ) ;
#19780 = ADVANCED_FACE ( 'NONE', ( #9133 ), #8922, .T. ) ;
#19779 = LINE ( 'NONE', #1082, #17469 ) ;
#19781 = DIRECTION ( 'NONE',  ( 0.000000000000000000, 0.000000000000000000, 1.000000000000000000 ) ) ;
#19782 = ORIENTED_EDGE ( 'NONE', *, *, #16879, .F. ) ;
#19783 = ORIENTED_EDGE ( 'NONE', *, *, #17881, .F. ) ;
#19784 = CARTESIAN_POINT ( 'NONE',  ( -15.21174975910705207, -51.86873716947361856, 68.00000000000000000 ) ) ;
#19785 = ADVANCED_FACE ( 'NONE', ( #14154 ), #4003, .T. ) ;
#19786 = PLANE ( 'NONE',  #3494 ) ;
#19787 = CARTESIAN_POINT ( 'NONE',  ( -23.06502549581203354, -2.381505846144857941, 13.31536975879940954 ) ) ;
#19788 = CARTESIAN_POINT ( 'NONE',  ( -1.824728116533986810, 42.36054587065083155, 49.66679706732590915 ) ) ;
#19789 = CARTESIAN_POINT ( 'NONE',  ( 28.87540678000427619, 0.000000000000000000, 7.799999999999999822 ) ) ;
#19790 = VERTEX_POINT ( 'NONE', #19425 ) ;
#19791 = CYLINDRICAL_SURFACE ( 'NONE', #13167, 0.2500000000000002220 ) ;
#19792 = CYLINDRICAL_SURFACE ( 'NONE', #19927, 0.04999999999999991257 ) ;
#19793 = CARTESIAN_POINT ( 'NONE',  ( -33.50000000000000000, -84.70000000000001705, 1.800000000000000266 ) ) ;
#19794 =( GEOMETRIC_REPRESENTATION_CONTEXT ( 3 ) GLOBAL_UNCERTAINTY_ASSIGNED_CONTEXT ( ( #17443 ) ) GLOBAL_UNIT_ASSIGNED_CONTEXT ( ( #5320, #11888, #1714 ) ) REPRESENTATION_CONTEXT ( 'NONE', 'WORKASPACE' ) );
#19795 = ORIENTED_EDGE ( 'NONE', *, *, #20857, .T. ) ;
#19796 = CARTESIAN_POINT ( 'NONE',  ( 1.724728116533979616, 43.31054587065082728, 43.75876104995653293 ) ) ;
#19797 = CARTESIAN_POINT ( 'NONE',  ( -34.39999999999999858, 85.00000000000000000, 0.6000000000000033085 ) ) ;
#19798 = EDGE_CURVE ( 'NONE', #8047, #1047, #19212, .T. ) ;
#19799 = FACE_OUTER_BOUND ( 'NONE', #1478, .T. ) ;
#19800 = VERTEX_POINT ( 'NONE', #621 ) ;
#19801 = EDGE_CURVE ( 'NONE', #11049, #15362, #4097, .T. ) ;
#19803 = CIRCLE ( 'NONE', #11924, 0.5000000000000004441 ) ;
#19802 = CARTESIAN_POINT ( 'NONE',  ( -1.724728116533986721, 43.31054587065082728, 31.80876104995653719 ) ) ;
#19804 = ORIENTED_EDGE ( 'NONE', *, *, #21671, .T. ) ;
#19805 = VERTEX_POINT ( 'NONE', #12474 ) ;
#19806 = VERTEX_POINT ( 'NONE', #399 ) ;
#19807 = DIRECTION ( 'NONE',  ( 0.000000000000000000, 0.000000000000000000, 1.000000000000000000 ) ) ;
#19808 = AXIS2_PLACEMENT_3D ( 'NONE', #15759, #9167, #18924 ) ;
#19809 = AXIS2_PLACEMENT_3D ( 'NONE', #16942, #16600, #1611 ) ;
#19810 = CARTESIAN_POINT ( 'NONE',  ( 33.49999999999999289, 84.70000000000001705, 1.500000000000001332 ) ) ;
#19811 = VERTEX_POINT ( 'NONE', #7476 ) ;
#19812 = CARTESIAN_POINT ( 'NONE',  ( -4.985331397971318523, 42.46645089659917716, 68.50000000000000000 ) ) ;
#19813 = EDGE_CURVE ( 'NONE', #4141, #8047, #8796, .T. ) ;
#19814 = DIRECTION ( 'NONE',  ( 0.000000000000000000, 1.000000000000000000, -0.000000000000000000 ) ) ;
#19815 = DIRECTION ( 'NONE',  ( 0.000000000000000000, 0.000000000000000000, 1.000000000000000000 ) ) ;
#19816 = EDGE_CURVE ( 'NONE', #19232, #2467, #15832, .T. ) ;
#19817 = CARTESIAN_POINT ( 'NONE',  ( 33.19999999999999574, 85.00000000000000000, 1.200000000000004174 ) ) ;
#19818 = CARTESIAN_POINT ( 'NONE',  ( 31.44597781366222122, 58.94165929845684104, 68.75000000000000000 ) ) ;
#19819 = DIRECTION ( 'NONE',  ( 0.000000000000000000, 0.000000000000000000, -1.000000000000000000 ) ) ;
#19820 = CYLINDRICAL_SURFACE ( 'NONE', #8301, 0.04999999999999991257 ) ;
#19821 = DIRECTION ( 'NONE',  ( 0.000000000000000000, 0.000000000000000000, 1.000000000000000000 ) ) ;
#19822 = CIRCLE ( 'NONE', #509, 0.2999999999999999334 ) ;
#19823 = ADVANCED_FACE ( 'NONE', ( #14273 ), #10818, .F. ) ;
#19824 = ORIENTED_EDGE ( 'NONE', *, *, #2127, .T. ) ;
#19825 = DIRECTION ( 'NONE',  ( -0.000000000000000000, -0.000000000000000000, -1.000000000000000000 ) ) ;
#19826 = B_SPLINE_CURVE_WITH_KNOTS ( 'NONE', 3,
 ( #19534, #14480, #5703, #12477, #4217, #9359, #12809, #11036, #9137, #10821, #16162, #19219 ),
 .UNSPECIFIED., .F., .F.,
 ( 4, 2, 2, 2, 2, 4 ),
 ( 0.000000000000000000, 0.0006847042422322843162, 0.001027056363348427667, 0.001198232423906498258, 0.001283820454185534638, 0.001369408484464571018 ),
 .UNSPECIFIED. ) ;
#19827 = EDGE_LOOP ( 'NONE', ( #17547, #2650, #21502, #6910, #9015, #8739 ) ) ;
#19828 = DIRECTION ( 'NONE',  ( 0.000000000000000000, 1.000000000000000000, 0.000000000000000000 ) ) ;
#19829 = CARTESIAN_POINT ( 'NONE',  ( -1.824728116533986810, 42.36054587065083155, 27.75876104995654003 ) ) ;
#19830 = UNCERTAINTY_MEASURE_WITH_UNIT (LENGTH_MEASURE( 1.000000000000000082E-05 ), #5293, 'distance_accuracy_value', 'NONE');
#19831 = ORIENTED_EDGE ( 'NONE', *, *, #517, .F. ) ;
#19832 = CARTESIAN_POINT ( 'NONE',  ( -1.824728116533986810, 43.31054587065082728, 35.80876104995653009 ) ) ;
#19833 = ORIENTED_EDGE ( 'NONE', *, *, #4260, .T. ) ;
#19834 = CIRCLE ( 'NONE', #7684, 5.000000000000000888 ) ;
#19835 = AXIS2_PLACEMENT_3D ( 'NONE', #21573, #19878, #19768 ) ;
#19836 = ORIENTED_EDGE ( 'NONE', *, *, #6134, .F. ) ;
#19837 = EDGE_CURVE ( 'NONE', #18477, #5820, #18808, .T. ) ;
#19838 = FACE_OUTER_BOUND ( 'NONE', #7592, .T. ) ;
#19839 = EDGE_CURVE ( 'NONE', #8243, #2243, #9158, .T. ) ;
#19840 = FACE_OUTER_BOUND ( 'NONE', #21657, .T. ) ;
#19841 = ORIENTED_EDGE ( 'NONE', *, *, #18803, .F. ) ;
#19842 = DIRECTION ( 'NONE',  ( 1.000000000000000000, 0.000000000000000000, 0.000000000000000000 ) ) ;
#19843 = FACE_OUTER_BOUND ( 'NONE', #12591, .T. ) ;
#19844 = DIRECTION ( 'NONE',  ( -6.751320378806396803E-15, -1.602473635475851075E-15, 1.000000000000000000 ) ) ;
#19845 = CARTESIAN_POINT ( 'NONE',  ( -23.02398829872513986, 2.157133568460765094, 13.26806292639400908 ) ) ;
#19846 = ORIENTED_EDGE ( 'NONE', *, *, #6956, .F. ) ;
#19847 = DIRECTION ( 'NONE',  ( 0.000000000000000000, 0.000000000000000000, 1.000000000000000000 ) ) ;
#19848 = CARTESIAN_POINT ( 'NONE',  ( -33.50000000000001421, -84.70000000000001705, 80.00000000000000000 ) ) ;
#19849 = VERTEX_POINT ( 'NONE', #2304 ) ;
#19850 = ORIENTED_EDGE ( 'NONE', *, *, #1162, .T. ) ;
#19851 = CIRCLE ( 'NONE', #4118, 0.5000000000000004441 ) ;
#19852 = ORIENTED_EDGE ( 'NONE', *, *, #356, .T. ) ;
#19853 = DIRECTION ( 'NONE',  ( 1.000000000000000000, 0.000000000000000000, 0.000000000000000000 ) ) ;
#19854 = FACE_OUTER_BOUND ( 'NONE', #10128, .T. ) ;
#19855 = VERTEX_POINT ( 'NONE', #7252 ) ;
#19856 = ADVANCED_FACE ( 'NONE', ( #503 ), #728, .T. ) ;
#19857 = DIRECTION ( 'NONE',  ( -0.000000000000000000, -0.000000000000000000, -1.000000000000000000 ) ) ;
#19858 = ORIENTED_EDGE ( 'NONE', *, *, #10121, .T. ) ;
#19859 = CARTESIAN_POINT ( 'NONE',  ( -27.67540678000428400, -36.74634676501047181, 13.50000000000000000 ) ) ;
#19860 = VECTOR ( 'NONE', #9965, 1000.000000000000000 ) ;
#19861 = LINE ( 'NONE', #4530, #20260 ) ;
#19862 = EDGE_CURVE ( 'NONE', #22112, #3651, #12021, .T. ) ;
#19863 = EDGE_CURVE ( 'NONE', #7977, #14982, #834, .T. ) ;
#19864 = CARTESIAN_POINT ( 'NONE',  ( 14.96174975910705918, 51.61873716947361856, 13.75000000000000000 ) ) ;
#19865 = DIRECTION ( 'NONE',  ( -1.000000000000000000, -0.000000000000000000, -6.123233995736764803E-17 ) ) ;
#19866 = CIRCLE ( 'NONE', #15203, 4.575000000000001066 ) ;
#19867 = DIRECTION ( 'NONE',  ( 0.000000000000000000, 0.000000000000000000, 1.000000000000000000 ) ) ;
#19868 = VECTOR ( 'NONE', #5441, 1000.000000000000000 ) ;
#19869 = FACE_OUTER_BOUND ( 'NONE', #17067, .T. ) ;
#19870 = CIRCLE ( 'NONE', #553, 0.2999999999999999334 ) ;
#19871 = ORIENTED_EDGE ( 'NONE', *, *, #6795, .T. ) ;
#19872 = CARTESIAN_POINT ( 'NONE',  ( -15.21174975910705207, 42.31054587065082728, 13.75000000000000000 ) ) ;
#19873 = DIRECTION ( 'NONE',  ( 0.9823853469773031755, -0.1868663427273193067, 0.000000000000000000 ) ) ;
#19874 = CARTESIAN_POINT ( 'NONE',  ( 33.19999999999999574, -84.70000000000001705, 78.20000000000000284 ) ) ;
#19875 = FACE_OUTER_BOUND ( 'NONE', #2215, .T. ) ;
#19876 = LINE ( 'NONE', #6346, #1514 ) ;
#19877 = EDGE_LOOP ( 'NONE', ( #15748, #392, #11966, #18818 ) ) ;
#19878 = DIRECTION ( 'NONE',  ( 0.000000000000000000, 1.000000000000000000, -0.000000000000000000 ) ) ;
#19879 = PLANE ( 'NONE',  #21842 ) ;
#19880 = APPLICATION_CONTEXT ( 'automotive_design' ) ;
#19881 = ORIENTED_EDGE ( 'NONE', *, *, #12281, .T. ) ;
#19882 = DIRECTION ( 'NONE',  ( 0.000000000000000000, 0.000000000000000000, -1.000000000000000000 ) ) ;
#19883 = DIRECTION ( 'NONE',  ( 0.000000000000000000, 0.000000000000000000, 1.000000000000000000 ) ) ;
#19884 = ORIENTED_EDGE ( 'NONE', *, *, #2170, .T. ) ;
#19885 = VECTOR ( 'NONE', #19705, 1000.000000000000000 ) ;
#19886 = CIRCLE ( 'NONE', #8097, 0.5000000000000000000 ) ;
#19887 = ORIENTED_EDGE ( 'NONE', *, *, #8509, .F. ) ;
#19888 = AXIS2_PLACEMENT_3D ( 'NONE', #17579, #18820, #2245 ) ;
#19889 = ORIENTED_EDGE ( 'NONE', *, *, #12686, .F. ) ;
#19890 = CARTESIAN_POINT ( 'NONE',  ( -29.50000000000002132, 69.00000000000000000, 0.2999999999999947153 ) ) ;
#19891 = DIRECTION ( 'NONE',  ( -0.000000000000000000, -0.000000000000000000, -1.000000000000000000 ) ) ;
#19892 = ADVANCED_FACE ( 'NONE', ( #4322 ), #2526, .T. ) ;
#19893 = DIRECTION ( 'NONE',  ( 0.000000000000000000, 0.000000000000000000, 1.000000000000000000 ) ) ;
#19894 = ORIENTED_EDGE ( 'NONE', *, *, #16224, .F. ) ;
#19895 = AXIS2_PLACEMENT_3D ( 'NONE', #4869, #8571, #6670 ) ;
#19896 = ORIENTED_EDGE ( 'NONE', *, *, #18027, .T. ) ;
#19897 = CARTESIAN_POINT ( 'NONE',  ( 31.50000000000002132, 71.00000000000001421, 3.200000000000000178 ) ) ;
#19898 = EDGE_CURVE ( 'NONE', #5647, #1165, #16666, .T. ) ;
#19899 = FACE_OUTER_BOUND ( 'NONE', #11831, .T. ) ;
#19900 = CARTESIAN_POINT ( 'NONE',  ( -29.17540678000427690, 0.000000000000000000, 7.500000000000000000 ) ) ;
#19901 = EDGE_CURVE ( 'NONE', #7269, #8930, #17412, .T. ) ;
#19902 = CARTESIAN_POINT ( 'NONE',  ( -25.37540678000429395, -38.74634676501045760, 13.79999999999999893 ) ) ;
#19903 = AXIS2_PLACEMENT_3D ( 'NONE', #16044, #5792, #21331 ) ;
#19904 = CONICAL_SURFACE ( 'NONE', #13088, 3077.683537175317724, 1.256637061435923464 ) ;
#19905 = CARTESIAN_POINT ( 'NONE',  ( -17.95292532278785913, -50.11873716947361856, 68.00000000000000000 ) ) ;
#19906 = CIRCLE ( 'NONE', #15235, 0.9652499999999990532 ) ;
#19907 = DIRECTION ( 'NONE',  ( 0.000000000000000000, 0.000000000000000000, -1.000000000000000000 ) ) ;
#19908 = ORIENTED_EDGE ( 'NONE', *, *, #11258, .T. ) ;
#19909 = CARTESIAN_POINT ( 'NONE',  ( 3.627054932750481964, 32.61873716947361856, 7.321391277662001151 ) ) ;
#19910 = CARTESIAN_POINT ( 'NONE',  ( -14.96174975910705207, -51.76873716947361714, 13.79999999999999716 ) ) ;
#19911 = LINE ( 'NONE', #4573, #1019 ) ;
#19912 = ORIENTED_EDGE ( 'NONE', *, *, #18814, .T. ) ;
#19913 = CARTESIAN_POINT ( 'NONE',  ( 9.141460742840918030, -32.93424481021354921, 13.50000000000000000 ) ) ;
#19914 = AXIS2_PLACEMENT_3D ( 'NONE', #7868, #12975, #4487 ) ;
#19915 = DIRECTION ( 'NONE',  ( -0.000000000000000000, 1.000000000000000000, -0.000000000000000000 ) ) ;
#19916 = FACE_OUTER_BOUND ( 'NONE', #11840, .T. ) ;
#19917 = ORIENTED_EDGE ( 'NONE', *, *, #12284, .F. ) ;
#19918 = FACE_OUTER_BOUND ( 'NONE', #21029, .T. ) ;
#19919 = EDGE_CURVE ( 'NONE', #6298, #19117, #20247, .T. ) ;
#19920 = LINE ( 'NONE', #20035, #2415 ) ;
#19921 = ORIENTED_EDGE ( 'NONE', *, *, #9098, .T. ) ;
#19922 = AXIS2_PLACEMENT_3D ( 'NONE', #21641, #2602, #12880 ) ;
#19923 = CIRCLE ( 'NONE', #12036, 0.5999999999999998668 ) ;
#19924 = AXIS2_PLACEMENT_3D ( 'NONE', #5280, #17230, #20715 ) ;
#19925 = ORIENTED_EDGE ( 'NONE', *, *, #10183, .F. ) ;
#19926 = CARTESIAN_POINT ( 'NONE',  ( -1.824728116533986810, 42.36054587065083155, 31.70876104995653932 ) ) ;
#19927 = AXIS2_PLACEMENT_3D ( 'NONE', #7947, #7706, #11267 ) ;
#19928 = AXIS2_PLACEMENT_3D ( 'NONE', #11555, #4755, #21880 ) ;
#19929 = EDGE_LOOP ( 'NONE', ( #9782, #13270, #19258, #16020 ) ) ;
#19930 = EDGE_CURVE ( 'NONE', #21823, #21318, #576, .T. ) ;
#19931 = FACE_OUTER_BOUND ( 'NONE', #8749, .T. ) ;
#19932 = ORIENTED_EDGE ( 'NONE', *, *, #8479, .F. ) ;
#19933 = DIRECTION ( 'NONE',  ( -1.000000000000000000, 0.000000000000000000, 0.000000000000000000 ) ) ;
#19934 = EDGE_CURVE ( 'NONE', #8611, #1327, #17369, .T. ) ;
#19935 = EDGE_CURVE ( 'NONE', #17488, #10373, #2005, .T. ) ;
#19936 = CARTESIAN_POINT ( 'NONE',  ( -1.724728116533986721, 43.26054587065083012, 29.71679706732590631 ) ) ;
#19937 = DIRECTION ( 'NONE',  ( 0.000000000000000000, 0.000000000000000000, 1.000000000000000000 ) ) ;
#19938 = CARTESIAN_POINT ( 'NONE',  ( 34.39999999999998437, -84.70000000000001705, 79.70000000000000284 ) ) ;
#19939 = TOROIDAL_SURFACE ( 'NONE', #9204, 6.800000000000001599, 0.2999999999999999889 ) ;
#19940 = AXIS2_PLACEMENT_3D ( 'NONE', #2122, #15656, #7283 ) ;
#19941 = CARTESIAN_POINT ( 'NONE',  ( -9.718906393579157310, 41.51128595893310802, 69.94509975324525897 ) ) ;
#19942 = DIRECTION ( 'NONE',  ( 0.000000000000000000, 0.000000000000000000, -1.000000000000000000 ) ) ;
#19943 = DIRECTION ( 'NONE',  ( -0.000000000000000000, 1.000000000000000000, -0.000000000000000000 ) ) ;
#19944 = DIRECTION ( 'NONE',  ( 0.000000000000000000, 0.000000000000000000, 1.000000000000000000 ) ) ;
#19945 = DIRECTION ( 'NONE',  ( 0.000000000000000000, 0.000000000000000000, -1.000000000000000000 ) ) ;
#19946 = TOROIDAL_SURFACE ( 'NONE', #10297, 1.500000000000000000, 0.5000000000000000000 ) ;
#19947 = CIRCLE ( 'NONE', #629, 0.05000000000000143219 ) ;
#19948 = ORIENTED_EDGE ( 'NONE', *, *, #17654, .T. ) ;
#19949 = FACE_OUTER_BOUND ( 'NONE', #268, .T. ) ;
#19950 = DIRECTION ( 'NONE',  ( 0.000000000000000000, 0.000000000000000000, 1.000000000000000000 ) ) ;
#19951 = EDGE_LOOP ( 'NONE', ( #15655, #9169, #8504, #9761 ) ) ;
#19952 = ORIENTED_EDGE ( 'NONE', *, *, #9949, .T. ) ;
#19953 = LINE ( 'NONE', #4618, #18887 ) ;
#19954 = EDGE_CURVE ( 'NONE', #9049, #11429, #15047, .T. ) ;
#19955 = CIRCLE ( 'NONE', #15991, 0.2500000000000002220 ) ;
#19956 = CIRCLE ( 'NONE', #3512, 0.05000000000000143219 ) ;
#19957 =( LENGTH_UNIT ( ) NAMED_UNIT ( * ) SI_UNIT ( .MILLI., .METRE. ) );
#19958 = ORIENTED_EDGE ( 'NONE', *, *, #12572, .T. ) ;
#19959 = ORIENTED_EDGE ( 'NONE', *, *, #5487, .F. ) ;
#19960 = AXIS2_PLACEMENT_3D ( 'NONE', #10181, #2289, #5269 ) ;
#19961 = ORIENTED_EDGE ( 'NONE', *, *, #3660, .F. ) ;
#19962 = AXIS2_PLACEMENT_3D ( 'NONE', #19420, #17732, #14470 ) ;
#19963 = EDGE_CURVE ( 'NONE', #12088, #4692, #18462, .T. ) ;
#19964 = CARTESIAN_POINT ( 'NONE',  ( -32.50000000000002132, 71.00000000000001421, 3.500000000000000000 ) ) ;
#19965 = LINE ( 'NONE', #18266, #21707 ) ;
#19966 = VERTEX_POINT ( 'NONE', #19995 ) ;
#19967 = SURFACE_STYLE_FILL_AREA ( #7988 ) ;
#19968 = DIRECTION ( 'NONE',  ( 0.000000000000000000, 1.000000000000000000, 0.000000000000000000 ) ) ;
#19969 = DIRECTION ( 'NONE',  ( 1.000000000000000000, 3.552713678800501718E-15, 0.000000000000000000 ) ) ;
#19970 = AXIS2_PLACEMENT_3D ( 'NONE', #5072, #6049, #7090 ) ;
#19971 = DIRECTION ( 'NONE',  ( -1.000000000000000000, 0.000000000000000000, 0.000000000000000000 ) ) ;
#19972 = ORIENTED_EDGE ( 'NONE', *, *, #2999, .T. ) ;
#19973 = DIRECTION ( 'NONE',  ( 1.000000000000000000, 0.000000000000000000, 0.000000000000000000 ) ) ;
#19974 = CIRCLE ( 'NONE', #18516, 0.2500000000000002220 ) ;
#19975 = ORIENTED_EDGE ( 'NONE', *, *, #9612, .T. ) ;
#19976 = AXIS2_PLACEMENT_3D ( 'NONE', #17366, #13679, #10348 ) ;
#19977 = ORIENTED_EDGE ( 'NONE', *, *, #12903, .F. ) ;
#19978 = AXIS2_PLACEMENT_3D ( 'NONE', #11176, #6173, #12621 ) ;
#19979 = ORIENTED_EDGE ( 'NONE', *, *, #1725, .T. ) ;
#19980 = CARTESIAN_POINT ( 'NONE',  ( 14.71174975910705740, 51.86873716947361856, 14.00000000000000000 ) ) ;
#19981 = TOROIDAL_SURFACE ( 'NONE', #13529, 0.05000000000000000278, 0.05000000000000000278 ) ;
#19983 = ADVANCED_FACE ( 'NONE', ( #6461 ), #6570, .F. ) ;
#19982 = CARTESIAN_POINT ( 'NONE',  ( -29.44760963940965226, -2.533475775848048617, 0.1250376690123979340 ) ) ;
#19984 = ORIENTED_EDGE ( 'NONE', *, *, #15383, .T. ) ;
#19985 = ADVANCED_FACE ( 'NONE', ( #13361 ), #14602, .T. ) ;
#19986 = FACE_OUTER_BOUND ( 'NONE', #16877, .T. ) ;
#19987 = ORIENTED_EDGE ( 'NONE', *, *, #16398, .F. ) ;
#19988 = DIRECTION ( 'NONE',  ( -0.000000000000000000, -1.000000000000000000, 0.000000000000000000 ) ) ;
#19989 = AXIS2_PLACEMENT_3D ( 'NONE', #14278, #21130, #12684 ) ;
#19990 = LINE ( 'NONE', #12910, #3832 ) ;
#19991 = CARTESIAN_POINT ( 'NONE',  ( 23.02398829872513630, -2.502141052783102726, 13.57900107139873214 ) ) ;
#19992 = CIRCLE ( 'NONE', #11397, 0.2999999999999999334 ) ;
#19993 = DIRECTION ( 'NONE',  ( 1.000000000000000000, -0.000000000000000000, 6.123233995736764803E-17 ) ) ;
#19994 = ORIENTED_EDGE ( 'NONE', *, *, #936, .T. ) ;
#19995 = CARTESIAN_POINT ( 'NONE',  ( 1.824728116533979261, 43.26054587065083012, 47.80876104995653719 ) ) ;
#19996 = DIRECTION ( 'NONE',  ( 0.000000000000000000, 0.000000000000000000, -1.000000000000000000 ) ) ;
#19997 = VECTOR ( 'NONE', #866, 1000.000000000000000 ) ;
#19998 = DIRECTION ( 'NONE',  ( 0.000000000000000000, 0.000000000000000000, 1.000000000000000000 ) ) ;
#19999 = DIRECTION ( 'NONE',  ( -0.9729678061520320442, -0.2309407893632090536, 0.000000000000000000 ) ) ;
#20000 = EDGE_LOOP ( 'NONE', ( #14031, #3248, #18363, #18145 ) ) ;
#20001 = EDGE_CURVE ( 'NONE', #18889, #6249, #20100, .T. ) ;
#20002 = DIRECTION ( 'NONE',  ( 1.000000000000000000, 0.000000000000000000, 6.123233995736764803E-17 ) ) ;
#20003 = CARTESIAN_POINT ( 'NONE',  ( -1.724728116533986721, 43.26054587065083012, 45.71679706732590631 ) ) ;
#20004 = ORIENTED_EDGE ( 'NONE', *, *, #11069, .T. ) ;
#20005 = DIRECTION ( 'NONE',  ( 0.000000000000000000, 0.000000000000000000, 1.000000000000000000 ) ) ;
#20006 = CARTESIAN_POINT ( 'NONE',  ( 30.79999999999999716, 69.70000000000000284, 1.200000000000003064 ) ) ;
#20007 = ORIENTED_EDGE ( 'NONE', *, *, #13987, .T. ) ;
#20008 = ORIENTED_EDGE ( 'NONE', *, *, #16104, .T. ) ;
#20009 = EDGE_LOOP ( 'NONE', ( #20118, #13637, #14337, #15276 ) ) ;
#20010 = DIRECTION ( 'NONE',  ( 0.000000000000000000, 1.000000000000000000, 0.000000000000000000 ) ) ;
#20011 = EDGE_CURVE ( 'NONE', #18383, #5113, #8114, .T. ) ;
#20012 = DIRECTION ( 'NONE',  ( -2.105859220307292343E-16, 1.000000000000000000, 0.000000000000000000 ) ) ;
#20013 = VECTOR ( 'NONE', #9750, 1000.000000000000000 ) ;
#20014 = ORIENTED_EDGE ( 'NONE', *, *, #13599, .T. ) ;
#20015 = VERTEX_POINT ( 'NONE', #946 ) ;
#20016 = FACE_OUTER_BOUND ( 'NONE', #20479, .T. ) ;
#20017 = CARTESIAN_POINT ( 'NONE',  ( 1.774728116533979660, 43.31054587065082728, 33.66679706732590915 ) ) ;
#20018 = DIRECTION ( 'NONE',  ( 0.000000000000000000, 0.000000000000000000, -1.000000000000000000 ) ) ;
#20019 = DIRECTION ( 'NONE',  ( 0.000000000000000000, 0.000000000000000000, 1.000000000000000000 ) ) ;
#20020 = DIRECTION ( 'NONE',  ( 0.000000000000000000, 0.000000000000000000, 1.000000000000000000 ) ) ;
#20021 = ORIENTED_EDGE ( 'NONE', *, *, #1756, .T. ) ;
#20022 = LINE ( 'NONE', #4689, #19250 ) ;
#20023 = EDGE_CURVE ( 'NONE', #9735, #4947, #11646, .T. ) ;
#20024 = AXIS2_PLACEMENT_3D ( 'NONE', #12708, #11388, #21485 ) ;
#20025 = VECTOR ( 'NONE', #8468, 1000.000000000000000 ) ;
#20026 = SPHERICAL_SURFACE ( 'NONE', #7415, 0.5000000000000000000 ) ;
#20027 = PRODUCT_DEFINITION_SHAPE ( 'NONE', 'NONE',  #22176 ) ;
#20028 = DIRECTION ( 'NONE',  ( -0.000000000000000000, -0.000000000000000000, -1.000000000000000000 ) ) ;
#20029 = EDGE_LOOP ( 'NONE', ( #5907, #16378, #7670, #13432 ) ) ;
#20030 = CARTESIAN_POINT ( 'NONE',  ( -34.70000000000001705, -84.70000000000001705, 80.00000000000000000 ) ) ;
#20031 = DIRECTION ( 'NONE',  ( 0.000000000000000000, 0.000000000000000000, -1.000000000000000000 ) ) ;
#20032 = ORIENTED_EDGE ( 'NONE', *, *, #2901, .F. ) ;
#20033 = FACE_OUTER_BOUND ( 'NONE', #12371, .T. ) ;
#20034 = ADVANCED_FACE ( 'NONE', ( #6231 ), #14814, .F. ) ;
#20035 = CARTESIAN_POINT ( 'NONE',  ( -8.638906393579159015, 44.91645089659918710, 70.88527860057354246 ) ) ;
#20036 = ORIENTED_EDGE ( 'NONE', *, *, #12619, .T. ) ;
#20037 = EDGE_CURVE ( 'NONE', #5989, #7404, #2632, .T. ) ;
#20038 = VERTEX_POINT ( 'NONE', #21456 ) ;
#20039 = CARTESIAN_POINT ( 'NONE',  ( 17.95292532278785913, -34.11873716947361856, 13.49999999999999822 ) ) ;
#20040 = AXIS2_PLACEMENT_3D ( 'NONE', #13585, #5200, #1724 ) ;
#20041 = VECTOR ( 'NONE', #9213, 1000.000000000000000 ) ;
#20042 = ORIENTED_EDGE ( 'NONE', *, *, #20598, .F. ) ;
#20043 = DIRECTION ( 'NONE',  ( 0.000000000000000000, 0.000000000000000000, 1.000000000000000000 ) ) ;
#20044 = DIRECTION ( 'NONE',  ( -1.000000000000000000, 0.000000000000000000, 0.000000000000000000 ) ) ;
#20045 = LINE ( 'NONE', #7631, #10585 ) ;
#20046 = LINE ( 'NONE', #18573, #6332 ) ;
#20047 = EDGE_CURVE ( 'NONE', #8820, #18590, #15593, .T. ) ;
#20048 = CARTESIAN_POINT ( 'NONE',  ( 23.07454441928563682, 2.431172533959870208, 13.33570496075367906 ) ) ;
#20049 = DIRECTION ( 'NONE',  ( 0.000000000000000000, 0.000000000000000000, 1.000000000000000000 ) ) ;
#20050 = VECTOR ( 'NONE', #2361, 1000.000000000000000 ) ;
#20051 = AXIS2_PLACEMENT_3D ( 'NONE', #7301, #21183, #4153 ) ;
#20052 = DIRECTION ( 'NONE',  ( 1.000000000000000000, 0.000000000000000000, 0.000000000000000000 ) ) ;
#20053 = DIRECTION ( 'NONE',  ( 1.000000000000000000, 0.000000000000000000, 0.000000000000000000 ) ) ;
#20054 = CARTESIAN_POINT ( 'NONE',  ( -1.724728116533986721, 43.26054587065083012, 31.80876104995653719 ) ) ;
#20055 = ADVANCED_FACE ( 'NONE', ( #4536 ), #932, .F. ) ;
#20056 = LINE ( 'NONE', #14358, #3478 ) ;
#20057 = ORIENTED_EDGE ( 'NONE', *, *, #20465, .F. ) ;
#20058 = CARTESIAN_POINT ( 'NONE',  ( -15.21174975910705207, 51.61873716947361856, 68.00000000000000000 ) ) ;
#20059 = EDGE_CURVE ( 'NONE', #10037, #5534, #19537, .T. ) ;
#20060 = EDGE_LOOP ( 'NONE', ( #10696, #6680, #7406, #17950 ) ) ;
#20061 = ORIENTED_EDGE ( 'NONE', *, *, #6466, .T. ) ;
#20062 = LINE ( 'NONE', #6197, #3874 ) ;
#20063 = EDGE_CURVE ( 'NONE', #17966, #12755, #11358, .T. ) ;
#20064 = CARTESIAN_POINT ( 'NONE',  ( -15.21174975910705207, -52.10286008774954780, 13.87500000000000000 ) ) ;
#20065 = ORIENTED_EDGE ( 'NONE', *, *, #17115, .F. ) ;
#20066 = ORIENTED_EDGE ( 'NONE', *, *, #16798, .T. ) ;
#20067 = AXIS2_PLACEMENT_3D ( 'NONE', #11923, #9932, #11708 ) ;
#20068 = EDGE_LOOP ( 'NONE', ( #18121, #20141, #4200, #15117 ) ) ;
#20069 = EDGE_CURVE ( 'NONE', #16873, #18705, #8816, .T. ) ;
#20070 = CARTESIAN_POINT ( 'NONE',  ( -3.127054932750481964, 32.93424481021354921, 68.50000000000000000 ) ) ;
#20071 = VECTOR ( 'NONE', #20973, 1000.000000000000000 ) ;
#20072 = TOROIDAL_SURFACE ( 'NONE', #20798, 0.05000000000000000278, 0.05000000000000000278 ) ;
#20073 = LINE ( 'NONE', #8545, #17105 ) ;
#20074 = ORIENTED_EDGE ( 'NONE', *, *, #21821, .T. ) ;
#20075 = DIRECTION ( 'NONE',  ( -0.000000000000000000, -0.000000000000000000, -1.000000000000000000 ) ) ;
#20076 = VECTOR ( 'NONE', #7892, 1000.000000000000000 ) ;
#20077 = DIRECTION ( 'NONE',  ( 1.224646799147353207E-16, 0.000000000000000000, 1.000000000000000000 ) ) ;
#20078 = AXIS2_PLACEMENT_3D ( 'NONE', #64, #5108, #20031 ) ;
#20079 = DIRECTION ( 'NONE',  ( 1.000000000000000000, 0.000000000000000000, 6.938893903907222067E-15 ) ) ;
#20080 = CARTESIAN_POINT ( 'NONE',  ( -28.90789898151107451, 6.496209923375007911, 7.643284004395015430 ) ) ;
#20081 = CARTESIAN_POINT ( 'NONE',  ( -15.95292532278785913, -50.11873716947361856, 68.00000000000000000 ) ) ;
#20082 = ADVANCED_FACE ( 'NONE', ( #10024 ), #1606, .T. ) ;
#20083 = VERTEX_POINT ( 'NONE', #15580 ) ;
#20084 = ORIENTED_EDGE ( 'NONE', *, *, #8562, .F. ) ;
#20085 = ORIENTED_EDGE ( 'NONE', *, *, #15798, .F. ) ;
#20086 = CARTESIAN_POINT ( 'NONE',  ( -30.07540678000427548, 0.000000000000000000, 7.200000000000000178 ) ) ;
#20087 = EDGE_CURVE ( 'NONE', #13533, #9687, #16289, .T. ) ;
#20088 = CARTESIAN_POINT ( 'NONE',  ( 29.20000000000002061, -2.799282752659324025, 0.000000000000000000 ) ) ;
#20089 = EDGE_LOOP ( 'NONE', ( #8666, #6837 ) ) ;
#20090 = AXIS2_PLACEMENT_3D ( 'NONE', #9247, #2523, #19422 ) ;
#20091 = CARTESIAN_POINT ( 'NONE',  ( 31.63662752439705272, 0.000000000000000000, 3.500000000000000000 ) ) ;
#20092 = AXIS2_PLACEMENT_3D ( 'NONE', #11088, #11419, #18132 ) ;
#20093 = VECTOR ( 'NONE', #17464, 1000.000000000000000 ) ;
#20094 = TOROIDAL_SURFACE ( 'NONE', #11846, 0.7000000000000000666, 0.2999999999999999889 ) ;
#20095 = ORIENTED_EDGE ( 'NONE', *, *, #9102, .T. ) ;
#20096 = LINE ( 'NONE', #17050, #13940 ) ;
#20097 = FACE_OUTER_BOUND ( 'NONE', #6364, .T. ) ;
#20098 = CARTESIAN_POINT ( 'NONE',  ( 0.000000000000000000, -69.04634676501045476, 3.500000000000000000 ) ) ;
#20099 = ORIENTED_EDGE ( 'NONE', *, *, #9098, .F. ) ;
#20100 = LINE ( 'NONE', #21567, #18090 ) ;
#20101 = CARTESIAN_POINT ( 'NONE',  ( -15.95292532278785913, 50.11873716947361856, 109.6002446535588319 ) ) ;
#20102 = ADVANCED_FACE ( 'NONE', ( #6904 ), #11789, .F. ) ;
#20103 = ADVANCED_FACE ( 'NONE', ( #3639 ), #9525, .T. ) ;
#20104 = DIRECTION ( 'NONE',  ( 1.000000000000000000, 0.000000000000000000, 0.000000000000000000 ) ) ;
#20105 = DIRECTION ( 'NONE',  ( -1.000000000000000000, 0.000000000000000000, 0.000000000000000000 ) ) ;
#20106 = ORIENTED_EDGE ( 'NONE', *, *, #17851, .F. ) ;
#20107 = DIRECTION ( 'NONE',  ( 0.000000000000000000, 0.000000000000000000, -1.000000000000000000 ) ) ;
#20108 = AXIS2_PLACEMENT_3D ( 'NONE', #15761, #3929, #5500 ) ;
#20109 = EDGE_LOOP ( 'NONE', ( #1257, #11672, #3787, #19717 ) ) ;
#20110 = FACE_OUTER_BOUND ( 'NONE', #2935, .T. ) ;
#20111 = VECTOR ( 'NONE', #2448, 1000.000000000000000 ) ;
#20112 = DIRECTION ( 'NONE',  ( 0.000000000000000000, -1.000000000000000000, 0.000000000000000000 ) ) ;
#20113 = VERTEX_POINT ( 'NONE', #8340 ) ;
#20114 = ORIENTED_EDGE ( 'NONE', *, *, #20490, .T. ) ;
#20115 = EDGE_LOOP ( 'NONE', ( #650, #6293, #18080, #13299 ) ) ;
#20116 = CARTESIAN_POINT ( 'NONE',  ( 14.71174975910705740, 51.61873716947361856, 13.75000000000000000 ) ) ;
#20117 = DIRECTION ( 'NONE',  ( -0.000000000000000000, 0.000000000000000000, 1.000000000000000000 ) ) ;
#20118 = ORIENTED_EDGE ( 'NONE', *, *, #865, .T. ) ;
#20119 = VECTOR ( 'NONE', #5854, 1000.000000000000000 ) ;
#20120 = EDGE_LOOP ( 'NONE', ( #4011, #12663, #22016, #4189 ) ) ;
#20121 = EDGE_CURVE ( 'NONE', #12842, #5989, #20314, .T. ) ;
#20122 = DIRECTION ( 'NONE',  ( -1.000000000000000000, 0.000000000000000000, 0.000000000000000000 ) ) ;
#20123 = DIRECTION ( 'NONE',  ( -1.000000000000000000, -0.000000000000000000, 0.000000000000000000 ) ) ;
#20124 = CARTESIAN_POINT ( 'NONE',  ( 30.07540678000427548, 0.000000000000000000, 7.200000000000000178 ) ) ;
#20125 = DIRECTION ( 'NONE',  ( -0.000000000000000000, 0.000000000000000000, 1.000000000000000000 ) ) ;
#20126 = DIRECTION ( 'NONE',  ( -0.000000000000000000, 0.000000000000000000, 1.000000000000000000 ) ) ;
#20127 = CARTESIAN_POINT ( 'NONE',  ( 1.724728116533979616, 43.31054587065082728, 31.70876104995653932 ) ) ;
#20128 = ORIENTED_EDGE ( 'NONE', *, *, #11516, .F. ) ;
#20129 = DIRECTION ( 'NONE',  ( 3.052134192567367925E-16, -1.000000000000000000, 0.000000000000000000 ) ) ;
#20130 = LINE ( 'NONE', #4906, #22066 ) ;
#20131 = EDGE_LOOP ( 'NONE', ( #4877, #1651, #4971, #11640 ) ) ;
#20132 = EDGE_CURVE ( 'NONE', #1026, #11756, #5331, .T. ) ;
#20133 = DIRECTION ( 'NONE',  ( 0.000000000000000000, -1.000000000000000000, 0.000000000000000000 ) ) ;
#20134 = CARTESIAN_POINT ( 'NONE',  ( 0.000000000000000000, -68.44634676501046044, 7.200000000000000178 ) ) ;
#20135 = ORIENTED_EDGE ( 'NONE', *, *, #9055, .T. ) ;
#20136 = CYLINDRICAL_SURFACE ( 'NONE', #6762, 0.3000000000000016542 ) ;
#20137 = DIRECTION ( 'NONE',  ( -6.123233995736764803E-17, 0.000000000000000000, 1.000000000000000000 ) ) ;
#20138 = EDGE_LOOP ( 'NONE', ( #12680, #3085, #20747, #21905 ) ) ;
#20139 = ORIENTED_EDGE ( 'NONE', *, *, #15442, .F. ) ;
#20140 = DIRECTION ( 'NONE',  ( 0.000000000000000000, 0.000000000000000000, 1.000000000000000000 ) ) ;
#20141 = ORIENTED_EDGE ( 'NONE', *, *, #10481, .T. ) ;
#20142 = EDGE_CURVE ( 'NONE', #13909, #4856, #6673, .T. ) ;
#20143 = CARTESIAN_POINT ( 'NONE',  ( -25.37540678000427263, -68.44634676501046044, 7.200000000000000178 ) ) ;
#20144 = DIRECTION ( 'NONE',  ( 1.000000000000000000, 0.000000000000000000, 0.000000000000000000 ) ) ;
#20145 = COLOUR_RGB ( '', 0.40784314, 0.44705882, 0.49803922) ;
#20146 = ADVANCED_FACE ( 'NONE', ( #15264 ), #8680, .T. ) ;
#20147 = DIRECTION ( 'NONE',  ( -1.000000000000000000, -0.000000000000000000, 0.000000000000000000 ) ) ;
#20148 = CARTESIAN_POINT ( 'NONE',  ( -27.67540678000428400, -36.74634676501047181, 13.79999999999999893 ) ) ;
#20149 = DIRECTION ( 'NONE',  ( 1.000000000000000000, 0.000000000000000000, 0.000000000000000000 ) ) ;
#20150 = DIRECTION ( 'NONE',  ( -0.1868663427273192512, -0.9823853469773029534, 0.000000000000000000 ) ) ;
#20151 = CARTESIAN_POINT ( 'NONE',  ( 17.92752199202934094, 38.74634676501045760, 13.79999999999999893 ) ) ;
#20152 = PLANE ( 'NONE',  #2944 ) ;
#20153 = DIRECTION ( 'NONE',  ( 0.000000000000000000, 0.000000000000000000, -1.000000000000000000 ) ) ;
#20154 = CARTESIAN_POINT ( 'NONE',  ( -32.23382792203229741, 83.71979900898287497, 68.50000000000000000 ) ) ;
#20155 = ORIENTED_EDGE ( 'NONE', *, *, #4879, .F. ) ;
#20156 = DIRECTION ( 'NONE',  ( 1.000000000000000000, 0.000000000000000000, 0.000000000000000000 ) ) ;
#20157 = CIRCLE ( 'NONE', #20529, 0.05000000000000143219 ) ;
#20158 = AXIS2_PLACEMENT_3D ( 'NONE', #11969, #11866, #1689 ) ;
#20159 = FACE_OUTER_BOUND ( 'NONE', #14615, .T. ) ;
#20160 = ORIENTED_EDGE ( 'NONE', *, *, #18965, .F. ) ;
#20161 = LINE ( 'NONE', #1573, #13171 ) ;
#20162 = ADVANCED_FACE ( 'NONE', ( #13591 ), #18513, .T. ) ;
#20163 = ORIENTED_EDGE ( 'NONE', *, *, #1696, .F. ) ;
#20164 = ORIENTED_EDGE ( 'NONE', *, *, #8002, .T. ) ;
#20165 = ORIENTED_EDGE ( 'NONE', *, *, #5700, .F. ) ;
#20166 = ORIENTED_EDGE ( 'NONE', *, *, #2240, .F. ) ;
#20167 = EDGE_CURVE ( 'NONE', #18383, #7934, #1303, .T. ) ;
#20168 = DIRECTION ( 'NONE',  ( 1.000000000000000000, 0.000000000000000000, 0.000000000000000000 ) ) ;
#20169 = EDGE_CURVE ( 'NONE', #18477, #10960, #1934, .T. ) ;
#20170 = CARTESIAN_POINT ( 'NONE',  ( 33.19999999999999574, -84.70000000000001705, 1.500000000000004219 ) ) ;
#20171 = ORIENTED_EDGE ( 'NONE', *, *, #9918, .T. ) ;
#20172 = FACE_OUTER_BOUND ( 'NONE', #4184, .T. ) ;
#20173 = EDGE_CURVE ( 'NONE', #7730, #1412, #231, .T. ) ;
#20174 = CARTESIAN_POINT ( 'NONE',  ( -23.02398829872514341, 2.876860926786018791, 13.71498478227948503 ) ) ;
#20175 = PLANE ( 'NONE',  #50 ) ;
#20176 = DIRECTION ( 'NONE',  ( 1.000000000000000000, 0.000000000000000000, 0.000000000000000000 ) ) ;
#20177 = DIRECTION ( 'NONE',  ( -1.224646799147353207E-16, -0.000000000000000000, -1.000000000000000000 ) ) ;
#20178 = EDGE_LOOP ( 'NONE', ( #16674, #7612, #17735, #16408 ) ) ;
#20179 = ORIENTED_EDGE ( 'NONE', *, *, #18856, .F. ) ;
#20180 = EDGE_LOOP ( 'NONE', ( #19145, #7931, #20559, #3820 ) ) ;
#20181 = DIRECTION ( 'NONE',  ( 1.000000000000000000, 0.000000000000000000, 0.000000000000000000 ) ) ;
#20182 = CARTESIAN_POINT ( 'NONE',  ( -9.641460742840918030, 32.93424481021354921, 68.50000000000000000 ) ) ;
#20183 = EDGE_CURVE ( 'NONE', #6210, #2269, #3105, .T. ) ;
#20184 = ORIENTED_EDGE ( 'NONE', *, *, #7705, .F. ) ;
#20185 = AXIS2_PLACEMENT_3D ( 'NONE', #15738, #739, #4012 ) ;
#20186 = DIRECTION ( 'NONE',  ( 0.8556185176499238043, 0.5176069476490315902, 0.000000000000000000 ) ) ;
#20187 = CIRCLE ( 'NONE', #9463, 0.2999999999999999334 ) ;
#20188 = PRODUCT_DEFINITION_SHAPE ( 'NONE', 'NONE',  #22170 ) ;
#20189 = EDGE_LOOP ( 'NONE', ( #11736, #5848, #21776, #16252 ) ) ;
#20190 = DIRECTION ( 'NONE',  ( 0.000000000000000000, 0.000000000000000000, 1.000000000000000000 ) ) ;
#20191 = DIRECTION ( 'NONE',  ( 0.000000000000000000, 1.000000000000000000, -0.000000000000000000 ) ) ;
#20192 = DIRECTION ( 'NONE',  ( 0.000000000000000000, 0.000000000000000000, 1.000000000000000000 ) ) ;
#20193 = ADVANCED_FACE ( 'NONE', ( #11900 ), #19662, .T. ) ;
#20194 = LINE ( 'NONE', #3637, #17363 ) ;
#20195 = VERTEX_POINT ( 'NONE', #15481 ) ;
#20196 = DIRECTION ( 'NONE',  ( 0.000000000000000000, -1.000000000000000000, 0.000000000000000000 ) ) ;
#20197 = EDGE_CURVE ( 'NONE', #17364, #16494, #14646, .T. ) ;
#20198 = DIRECTION ( 'NONE',  ( 0.000000000000000000, -0.000000000000000000, -1.000000000000000000 ) ) ;
#20199 = CARTESIAN_POINT ( 'NONE',  ( 14.71174975910707161, 0.000000000000000000, 68.50000000000000000 ) ) ;
#20200 = CARTESIAN_POINT ( 'NONE',  ( -1.724728116533986721, 42.36054587065083155, 53.71679706732590631 ) ) ;
#20201 = CARTESIAN_POINT ( 'NONE',  ( -8.638906393579159015, 43.51045099701597252, 68.06527860057354928 ) ) ;
#20202 = ORIENTED_EDGE ( 'NONE', *, *, #12421, .T. ) ;
#20203 = PLANE ( 'NONE',  #10566 ) ;
#20204 = AXIS2_PLACEMENT_3D ( 'NONE', #7011, #13919, #9109 ) ;
#20205 = VECTOR ( 'NONE', #18067, 1000.000000000000000 ) ;
#20206 = ORIENTED_EDGE ( 'NONE', *, *, #3235, .F. ) ;
#20207 = DIRECTION ( 'NONE',  ( 0.000000000000000000, 0.000000000000000000, -1.000000000000000000 ) ) ;
#20208 = CARTESIAN_POINT ( 'NONE',  ( 30.37540678000427619, -6.000000000000000000, 7.500000000000000000 ) ) ;
#20209 = ORIENTED_EDGE ( 'NONE', *, *, #2205, .T. ) ;
#20210 = EDGE_LOOP ( 'NONE', ( #1981, #21379, #5107, #21720 ) ) ;
#20211 = VERTEX_POINT ( 'NONE', #54 ) ;
#20212 = DIRECTION ( 'NONE',  ( 0.000000000000000000, 0.000000000000000000, 1.000000000000000000 ) ) ;
#20213 = FACE_OUTER_BOUND ( 'NONE', #9947, .T. ) ;
#20214 = EDGE_LOOP ( 'NONE', ( #1296, #18364, #2074, #20638 ) ) ;
#20215 = DIRECTION ( 'NONE',  ( -1.000000000000000000, 0.000000000000000000, 0.000000000000000000 ) ) ;
#20216 = ORIENTED_EDGE ( 'NONE', *, *, #20786, .T. ) ;
#20217 = EDGE_CURVE ( 'NONE', #13749, #16971, #6452, .T. ) ;
#20218 = VERTEX_POINT ( 'NONE', #4178 ) ;
#20219 = CARTESIAN_POINT ( 'NONE',  ( -25.37540678000427263, -63.74634676501045050, 7.200000000000000178 ) ) ;
#20220 = CIRCLE ( 'NONE', #18797, 2.500000000000000444 ) ;
#20221 = CIRCLE ( 'NONE', #3790, 0.2999999999999999334 ) ;
#20222 = CIRCLE ( 'NONE', #18420, 0.2999999999999999334 ) ;
#20223 = CARTESIAN_POINT ( 'NONE',  ( 3.127054932750481964, -32.61873716947361856, 68.00000000000000000 ) ) ;
#20224 = CARTESIAN_POINT ( 'NONE',  ( -23.02398829872513986, -3.395978615688242996, 13.79999998357615532 ) ) ;
#20225 = DIRECTION ( 'NONE',  ( 0.000000000000000000, 1.000000000000000000, 0.000000000000000000 ) ) ;
#20226 = CARTESIAN_POINT ( 'NONE',  ( -15.95292532278785913, -34.11873716947361856, 68.00000000000000000 ) ) ;
#20227 = DIRECTION ( 'NONE',  ( 1.000000000000000000, 0.000000000000000000, 0.000000000000000000 ) ) ;
#20228 = EDGE_CURVE ( 'NONE', #19432, #4119, #5024, .T. ) ;
#20229 = FACE_OUTER_BOUND ( 'NONE', #15668, .T. ) ;
#20230 = DIRECTION ( 'NONE',  ( -0.000000000000000000, 1.000000000000000000, -0.000000000000000000 ) ) ;
#20231 = CYLINDRICAL_SURFACE ( 'NONE', #3885, 2.500000000000002220 ) ;
#20232 = ORIENTED_EDGE ( 'NONE', *, *, #19757, .F. ) ;
#20233 = VECTOR ( 'NONE', #788, 1000.000000000000000 ) ;
#20234 = AXIS2_PLACEMENT_3D ( 'NONE', #21883, #4757, #13246 ) ;
#20235 = CARTESIAN_POINT ( 'NONE',  ( 1.724728116533979838, 43.26054587065083012, 49.66679706732590915 ) ) ;
#20236 = VECTOR ( 'NONE', #8414, 1000.000000000000000 ) ;
#20237 = ORIENTED_EDGE ( 'NONE', *, *, #16088, .T. ) ;
#20238 = AXIS2_PLACEMENT_3D ( 'NONE', #17899, #1002, #13203 ) ;
#20239 = AXIS2_PLACEMENT_3D ( 'NONE', #21094, #10460, #19495 ) ;
#20240 = DIRECTION ( 'NONE',  ( -0.000000000000000000, -1.000000000000000000, 0.000000000000000000 ) ) ;
#20241 = DIRECTION ( 'NONE',  ( 0.000000000000000000, 0.000000000000000000, 1.000000000000000000 ) ) ;
#20242 = ORIENTED_EDGE ( 'NONE', *, *, #6942, .F. ) ;
#20243 = ORIENTED_EDGE ( 'NONE', *, *, #17595, .T. ) ;
#20244 = FACE_OUTER_BOUND ( 'NONE', #15774, .T. ) ;
#20245 = EDGE_CURVE ( 'NONE', #3082, #12310, #472, .T. ) ;
#20246 = EDGE_CURVE ( 'NONE', #9769, #706, #3585, .T. ) ;
#20247 = CIRCLE ( 'NONE', #21324, 0.05000000000000143219 ) ;
#20248 = VECTOR ( 'NONE', #6682, 1000.000000000000000 ) ;
#20249 = AXIS2_PLACEMENT_3D ( 'NONE', #9301, #16105, #787 ) ;
#20250 = CARTESIAN_POINT ( 'NONE',  ( -13.75390639357915923, 42.46645089659918426, 70.38908280829822672 ) ) ;
#20251 = ORIENTED_EDGE ( 'NONE', *, *, #18049, .T. ) ;
#20252 = DIRECTION ( 'NONE',  ( -0.000000000000000000, -0.000000000000000000, -1.000000000000000000 ) ) ;
#20253 = VECTOR ( 'NONE', #8079, 1000.000000000000000 ) ;
#20254 = DIRECTION ( 'NONE',  ( 1.000000000000000000, 0.000000000000000000, -2.546383084002652634E-16 ) ) ;
#20255 = DIRECTION ( 'NONE',  ( 0.000000000000000000, -1.000000000000000000, 0.000000000000000000 ) ) ;
#20256 = DIRECTION ( 'NONE',  ( -0.000000000000000000, -1.000000000000000000, -0.000000000000000000 ) ) ;
#20257 = DIRECTION ( 'NONE',  ( 1.000000000000000000, 0.000000000000000000, 0.000000000000000000 ) ) ;
#20258 = DIRECTION ( 'NONE',  ( -1.000000000000000000, 0.000000000000000000, 0.000000000000000000 ) ) ;
#20259 = DIRECTION ( 'NONE',  ( 0.000000000000000000, -0.000000000000000000, -1.000000000000000000 ) ) ;
#20260 = VECTOR ( 'NONE', #9692, 1000.000000000000000 ) ;
#20262 = EDGE_CURVE ( 'NONE', #12734, #21299, #1801, .T. ) ;
#20261 = DIRECTION ( 'NONE',  ( 1.000000000000000000, 0.000000000000000000, 0.000000000000000000 ) ) ;
#20263 = TOROIDAL_SURFACE ( 'NONE', #22064, 0.7000000000000000666, 0.2999999999999999889 ) ;
#20264 = AXIS2_PLACEMENT_3D ( 'NONE', #17280, #12660, #21211 ) ;
#20265 = VECTOR ( 'NONE', #9387, 1000.000000000000000 ) ;
#20266 = CARTESIAN_POINT ( 'NONE',  ( 4.127054932750481520, 33.93424481021354921, 68.00000000000000000 ) ) ;
#20267 = ORIENTED_EDGE ( 'NONE', *, *, #12218, .F. ) ;
#20268 = CARTESIAN_POINT ( 'NONE',  ( -15.95292532278785913, -50.11873716947361856, 13.99999999999999822 ) ) ;
#20269 = VERTEX_POINT ( 'NONE', #15803 ) ;
#20270 = AXIS2_PLACEMENT_3D ( 'NONE', #6361, #16278, #9470 ) ;
#20271 = ORIENTED_EDGE ( 'NONE', *, *, #20574, .T. ) ;
#20272 = DIRECTION ( 'NONE',  ( -1.000000000000000000, -0.000000000000000000, -0.000000000000000000 ) ) ;
#20273 = DIRECTION ( 'NONE',  ( 0.000000000000000000, 0.000000000000000000, 1.000000000000000000 ) ) ;
#20274 = EDGE_CURVE ( 'NONE', #8409, #17039, #4668, .T. ) ;
#20275 = ORIENTED_EDGE ( 'NONE', *, *, #3471, .T. ) ;
#20276 =( NAMED_UNIT ( * ) PLANE_ANGLE_UNIT ( ) SI_UNIT ( $, .RADIAN. ) );
#20277 = VERTEX_POINT ( 'NONE', #11000 ) ;
#20278 = AXIS2_PLACEMENT_3D ( 'NONE', #10077, #12065, #11952 ) ;
#20279 = AXIS2_PLACEMENT_3D ( 'NONE', #11173, #1201, #7953 ) ;
#20280 = VERTEX_POINT ( 'NONE', #7221 ) ;
#20281 = DIRECTION ( 'NONE',  ( 1.000000000000000000, 3.387630566026860322E-15, -1.224646799147353207E-16 ) ) ;
#20282 = DIRECTION ( 'NONE',  ( 6.123233995736764803E-17, 0.000000000000000000, -1.000000000000000000 ) ) ;
#20283 = VECTOR ( 'NONE', #2698, 1000.000000000000000 ) ;
#20284 = CYLINDRICAL_SURFACE ( 'NONE', #4951, 0.3000000000000016542 ) ;
#20285 = VECTOR ( 'NONE', #713, 1000.000000000000000 ) ;
#20286 = ORIENTED_EDGE ( 'NONE', *, *, #19935, .T. ) ;
#20287 = AXIS2_PLACEMENT_3D ( 'NONE', #17077, #18410, #13162 ) ;
#20288 = ADVANCED_FACE ( 'NONE', ( #7437 ), #14018, .T. ) ;
#20289 = LINE ( 'NONE', #132, #21194 ) ;
#20290 = PLANE ( 'NONE',  #8998 ) ;
#20291 = DIRECTION ( 'NONE',  ( 0.000000000000000000, 0.000000000000000000, -1.000000000000000000 ) ) ;
#20292 = AXIS2_PLACEMENT_3D ( 'NONE', #8287, #21937, #6613 ) ;
#20293 = VERTEX_POINT ( 'NONE', #19397 ) ;
#20294 = CIRCLE ( 'NONE', #20674, 0.04999999999999991257 ) ;
#20295 = CIRCLE ( 'NONE', #10647, 0.3000000000000016542 ) ;
#20296 = ORIENTED_EDGE ( 'NONE', *, *, #19603, .T. ) ;
#20297 = ORIENTED_EDGE ( 'NONE', *, *, #15335, .T. ) ;
#20298 = LINE ( 'NONE', #21879, #8141 ) ;
#20299 = EDGE_CURVE ( 'NONE', #16703, #12463, #2497, .T. ) ;
#20300 = DIRECTION ( 'NONE',  ( -0.000000000000000000, 1.000000000000000000, -0.000000000000000000 ) ) ;
#20301 = EDGE_CURVE ( 'NONE', #18477, #8820, #3598, .T. ) ;
#20302 = EDGE_CURVE ( 'NONE', #17392, #7401, #4068, .T. ) ;
#20303 = VECTOR ( 'NONE', #2556, 1000.000000000000000 ) ;
#20304 = DIRECTION ( 'NONE',  ( 1.000000000000000000, 0.000000000000000000, 0.000000000000000000 ) ) ;
#20305 = AXIS2_PLACEMENT_3D ( 'NONE', #6087, #11095, #11200 ) ;
#20306 = AXIS2_PLACEMENT_3D ( 'NONE', #16, #17132, #1804 ) ;
#20307 = ORIENTED_EDGE ( 'NONE', *, *, #20928, .T. ) ;
#20308 = DIRECTION ( 'NONE',  ( 0.000000000000000000, 1.000000000000000000, 0.000000000000000000 ) ) ;
#20309 = LINE ( 'NONE', #148, #14519 ) ;
#20310 = DIRECTION ( 'NONE',  ( -1.000000000000000000, 1.788744114411106313E-17, -6.123233995736764803E-17 ) ) ;
#20311 = CIRCLE ( 'NONE', #9539, 3.200000000000001510 ) ;
#20312 = DIRECTION ( 'NONE',  ( -0.2309407893632116904, 0.9729678061520312671, 0.000000000000000000 ) ) ;
#20313 = ORIENTED_EDGE ( 'NONE', *, *, #9739, .T. ) ;
#20314 = LINE ( 'NONE', #13688, #12362 ) ;
#20315 = LINE ( 'NONE', #4767, #9969 ) ;
#20316 = EDGE_CURVE ( 'NONE', #16789, #17520, #16131, .T. ) ;
#20317 = CARTESIAN_POINT ( 'NONE',  ( 0.000000000000000000, 51.61873716947361856, 68.00000000000000000 ) ) ;
#20318 = VECTOR ( 'NONE', #1872, 1000.000000000000000 ) ;
#20319 = CARTESIAN_POINT ( 'NONE',  ( -1.724728116533986721, 43.26054587065083012, 29.76679706732590702 ) ) ;
#20320 = CARTESIAN_POINT ( 'NONE',  ( 0.000000000000000000, -38.74634676501045760, 42.50000000000000000 ) ) ;
#20321 = ORIENTED_EDGE ( 'NONE', *, *, #5988, .T. ) ;
#20322 = FACE_OUTER_BOUND ( 'NONE', #21212, .T. ) ;
#20323 = CIRCLE ( 'NONE', #14901, 0.1000000000000028644 ) ;
#20324 = CIRCLE ( 'NONE', #19253, 0.5000000000000004441 ) ;
#20325 = AXIS2_PLACEMENT_3D ( 'NONE', #16642, #1538, #18439 ) ;
#20326 = VERTEX_POINT ( 'NONE', #10885 ) ;
#20327 = CARTESIAN_POINT ( 'NONE',  ( 23.32398829872514412, -5.683640910026986681, 13.79999999999999893 ) ) ;
#20328 = DIRECTION ( 'NONE',  ( 0.000000000000000000, -0.000000000000000000, 1.000000000000000000 ) ) ;
#20329 = EDGE_LOOP ( 'NONE', ( #20202, #13224, #8307, #20899 ) ) ;
#20330 = VERTEX_POINT ( 'NONE', #369 ) ;
#20331 = ORIENTED_EDGE ( 'NONE', *, *, #7860, .T. ) ;
#20332 = LINE ( 'NONE', #15396, #18471 ) ;
#20333 = ADVANCED_FACE ( 'NONE', ( #9323, #21203, #12320, #809 ), #10558, .T. ) ;
#20334 = DIRECTION ( 'NONE',  ( 0.000000000000000000, 0.000000000000000000, -1.000000000000000000 ) ) ;
#20335 = ADVANCED_FACE ( 'NONE', ( #17377 ), #20971, .T. ) ;
#20336 = VECTOR ( 'NONE', #2531, 1000.000000000000000 ) ;
#20337 = VERTEX_POINT ( 'NONE', #10789 ) ;
#20338 = FACE_OUTER_BOUND ( 'NONE', #1629, .T. ) ;
#20339 = EDGE_CURVE ( 'NONE', #16591, #20218, #18947, .T. ) ;
#20340 = EDGE_LOOP ( 'NONE', ( #14068, #18317, #17569, #6201 ) ) ;
#20341 = VECTOR ( 'NONE', #18626, 1000.000000000000000 ) ;
#20342 = ORIENTED_EDGE ( 'NONE', *, *, #18443, .F. ) ;
#20343 = LINE ( 'NONE', #6820, #17857 ) ;
#20344 = AXIS2_PLACEMENT_3D ( 'NONE', #12696, #21243, #9263 ) ;
#20345 = VERTEX_POINT ( 'NONE', #20759 ) ;
#20346 = DIRECTION ( 'NONE',  ( -1.000000000000000000, 0.000000000000000000, 0.000000000000000000 ) ) ;
#20347 = DIRECTION ( 'NONE',  ( 0.000000000000000000, -0.000000000000000000, 1.000000000000000000 ) ) ;
#20348 = DIRECTION ( 'NONE',  ( -0.000000000000000000, -1.000000000000000000, -0.000000000000000000 ) ) ;
#20349 = CARTESIAN_POINT ( 'NONE',  ( 1.774728116533979660, 43.26054587065083012, 51.80876104995653719 ) ) ;
#20350 = ORIENTED_EDGE ( 'NONE', *, *, #21991, .F. ) ;
#20351 = CARTESIAN_POINT ( 'NONE',  ( 0.000000000000000000, 69.04634676501045476, 3.799999999999999822 ) ) ;
#20352 = CARTESIAN_POINT ( 'NONE',  ( -9.141460742840918030, -32.93424481021354921, 42.50000000000000000 ) ) ;
#20353 = EDGE_CURVE ( 'NONE', #6383, #15755, #17517, .T. ) ;
#20354 = ADVANCED_BREP_SHAPE_REPRESENTATION ( '', ( #20594, #17493 ), #6222 ) ;
#20355 = DIRECTION ( 'NONE',  ( 0.000000000000000000, 1.000000000000000000, -1.084202172485523564E-15 ) ) ;
#20356 = DIRECTION ( 'NONE',  ( -1.000000000000000000, 0.000000000000000000, -8.673617379884034239E-17 ) ) ;
#20357 = EDGE_LOOP ( 'NONE', ( #3459, #9817, #18186, #21554 ) ) ;
#20358 = DIRECTION ( 'NONE',  ( -1.000000000000000000, 0.000000000000000000, 0.000000000000000000 ) ) ;
#20359 = EDGE_CURVE ( 'NONE', #15132, #1577, #12552, .T. ) ;
#20360 = CIRCLE ( 'NONE', #16413, 1.000000000000000888 ) ;
#20361 = FACE_OUTER_BOUND ( 'NONE', #11482, .T. ) ;
#20362 = ORIENTED_EDGE ( 'NONE', *, *, #2252, .F. ) ;
#20363 = CARTESIAN_POINT ( 'NONE',  ( -1.824728116533986810, 43.31054587065082728, 35.70876104995653577 ) ) ;
#20364 = DIRECTION ( 'NONE',  ( 0.000000000000000000, -0.000000000000000000, -1.000000000000000000 ) ) ;
#20365 = ORIENTED_EDGE ( 'NONE', *, *, #11090, .F. ) ;
#20366 = ORIENTED_EDGE ( 'NONE', *, *, #9180, .T. ) ;
#20367 = DIRECTION ( 'NONE',  ( 0.000000000000000000, 0.000000000000000000, -1.000000000000000000 ) ) ;
#20368 = EDGE_CURVE ( 'NONE', #8087, #9625, #2841, .T. ) ;
#20369 = ORIENTED_EDGE ( 'NONE', *, *, #12512, .T. ) ;
#20370 = AXIS2_PLACEMENT_3D ( 'NONE', #373, #17607, #5439 ) ;
#20371 = CARTESIAN_POINT ( 'NONE',  ( -9.178906393579158163, 42.46645089659918426, 67.75164986378473486 ) ) ;
#20372 = CIRCLE ( 'NONE', #16426, 2.000000000000001776 ) ;
#20373 = ORIENTED_EDGE ( 'NONE', *, *, #11791, .F. ) ;
#20374 = DIRECTION ( 'NONE',  ( 6.123233995736764803E-17, 0.000000000000000000, -1.000000000000000000 ) ) ;
#20375 = COLOUR_RGB ( '', 0.31764706, 0.68627451, 0.89019608) ;
#20376 = VECTOR ( 'NONE', #15819, 1000.000000000000000 ) ;
#20377 = CARTESIAN_POINT ( 'NONE',  ( -1.824728116533986810, 43.31054587065082728, 51.80876104995653719 ) ) ;
#20378 = DIRECTION ( 'NONE',  ( -0.9729678061520345977, -0.2309407893631976461, 0.000000000000000000 ) ) ;
#20379 = CYLINDRICAL_SURFACE ( 'NONE', #1774, 0.5000000000000004441 ) ;
#20380 = DIRECTION ( 'NONE',  ( 0.000000000000000000, 0.000000000000000000, -1.000000000000000000 ) ) ;
#20381 = EDGE_CURVE ( 'NONE', #11094, #1177, #18154, .T. ) ;
#20382 = FACE_OUTER_BOUND ( 'NONE', #1185, .T. ) ;
#20383 = EDGE_CURVE ( 'NONE', #1923, #9228, #21448, .T. ) ;
#20384 = LINE ( 'NONE', #15441, #15781 ) ;
#20385 = EDGE_CURVE ( 'NONE', #8021, #17208, #13583, .T. ) ;
#20386 = CARTESIAN_POINT ( 'NONE',  ( 30.50000000000000000, -84.70000000000001705, 4.011548038196366406E-15 ) ) ;
#20387 = AXIS2_PLACEMENT_3D ( 'NONE', #11126, #19988, #9691 ) ;
#20388 = ORIENTED_EDGE ( 'NONE', *, *, #1281, .T. ) ;
#20389 = DIRECTION ( 'NONE',  ( -1.000000000000000000, 0.000000000000000000, -0.000000000000000000 ) ) ;
#20390 = ORIENTED_EDGE ( 'NONE', *, *, #13104, .T. ) ;
#20391 = DIRECTION ( 'NONE',  ( -1.000000000000000000, 0.000000000000000000, 0.000000000000000000 ) ) ;
#20392 = PRODUCT ( 'Flap', 'Flap', '', ( #12407 ) ) ;
#20393 = VERTEX_POINT ( 'NONE', #4742 ) ;
#20394 = ORIENTED_EDGE ( 'NONE', *, *, #16209, .F. ) ;
#20395 = DIRECTION ( 'NONE',  ( 1.000000000000000000, 0.000000000000000000, 0.000000000000000000 ) ) ;
#20396 = PRODUCT_CONTEXT ( 'NONE', #17584, 'mechanical' ) ;
#20397 = EDGE_LOOP ( 'NONE', ( #4390, #10958, #6655, #15474 ) ) ;
#20398 = ORIENTED_EDGE ( 'NONE', *, *, #7203, .T. ) ;
#20399 = ORIENTED_EDGE ( 'NONE', *, *, #18247, .F. ) ;
#20400 = EDGE_CURVE ( 'NONE', #4089, #8303, #17160, .T. ) ;
#20401 = ORIENTED_EDGE ( 'NONE', *, *, #11112, .F. ) ;
#20402 = AXIS2_PLACEMENT_3D ( 'NONE', #4201, #11022, #17842 ) ;
#20403 = CARTESIAN_POINT ( 'NONE',  ( 1.774728116533979438, 43.31054587065082728, 43.80876104995653719 ) ) ;
#20404 = AXIS2_PLACEMENT_3D ( 'NONE', #21867, #15026, #3282 ) ;
#20405 = CARTESIAN_POINT ( 'NONE',  ( -1.836970198721029934E-16, -72.00000000000001421, 3.500000000000000000 ) ) ;
#20406 = EDGE_LOOP ( 'NONE', ( #7848, #17218, #10822, #18768 ) ) ;
#20407 = FACE_OUTER_BOUND ( 'NONE', #4080, .T. ) ;
#20408 = EDGE_CURVE ( 'NONE', #3983, #12670, #7532, .T. ) ;
#20409 = DIRECTION ( 'NONE',  ( 1.000000000000000000, -3.052134192567374827E-16, 0.000000000000000000 ) ) ;
#20410 = DIRECTION ( 'NONE',  ( 1.000000000000000000, 2.832483164223420229E-16, 0.000000000000000000 ) ) ;
#20411 = EDGE_CURVE ( 'NONE', #16033, #19805, #21539, .T. ) ;
#20412 = CARTESIAN_POINT ( 'NONE',  ( 29.37540678000427619, -6.000000000000000000, 3.799999999999999822 ) ) ;
#20413 = CARTESIAN_POINT ( 'NONE',  ( 15.95292532278785913, 50.11873716947361856, 13.99999999999999822 ) ) ;
#20414 = ORIENTED_EDGE ( 'NONE', *, *, #21721, .F. ) ;
#20415 = MANIFOLD_SOLID_BREP ( 'Stock-MAS-696-1', #264 ) ;
#20416 = EDGE_LOOP ( 'NONE', ( #14212, #8906, #21214, #16839 ) ) ;
#20417 = ORIENTED_EDGE ( 'NONE', *, *, #14359, .T. ) ;
#20418 = DIRECTION ( 'NONE',  ( 0.000000000000000000, 0.000000000000000000, 1.000000000000000000 ) ) ;
#20419 = CARTESIAN_POINT ( 'NONE',  ( -29.33570773061603276, -2.657594995084290979, 0.02220324760240992637 ) ) ;
#20420 = ORIENTED_EDGE ( 'NONE', *, *, #4381, .F. ) ;
#20421 = VECTOR ( 'NONE', #18575, 1000.000000000000000 ) ;
#20422 = FACE_OUTER_BOUND ( 'NONE', #18378, .T. ) ;
#20423 = VERTEX_POINT ( 'NONE', #4397 ) ;
#20424 = DIRECTION ( 'NONE',  ( 0.000000000000000000, 0.000000000000000000, 1.000000000000000000 ) ) ;
#20425 = VECTOR ( 'NONE', #8685, 1000.000000000000000 ) ;
#20426 = LINE ( 'NONE', #5095, #4538 ) ;
#20427 = VECTOR ( 'NONE', #592, 1000.000000000000000 ) ;
#20428 = DIRECTION ( 'NONE',  ( 1.000000000000000000, 0.000000000000000000, 0.000000000000000000 ) ) ;
#20429 = EDGE_LOOP ( 'NONE', ( #138, #6637, #1723, #3850 ) ) ;
#20430 = CARTESIAN_POINT ( 'NONE',  ( 0.000000000000000000, -32.61873716947361856, 68.00000000000000000 ) ) ;
#20431 = CARTESIAN_POINT ( 'NONE',  ( 1.824728116533979261, 43.26054587065083012, 35.80876104995653009 ) ) ;
#20432 = ADVANCED_FACE ( 'NONE', ( #2713 ), #4631, .T. ) ;
#20433 = CARTESIAN_POINT ( 'NONE',  ( 27.67540678000427690, 10.94079601157914539, 13.50000000000000000 ) ) ;
#20434 = EDGE_CURVE ( 'NONE', #5130, #16130, #13233, .T. ) ;
#20435 = CARTESIAN_POINT ( 'NONE',  ( -21.92816239687475743, 42.46645089659918426, 68.25000000000000000 ) ) ;
#20436 = CARTESIAN_POINT ( 'NONE',  ( -29.13662752439705272, 5.000000000000000000, 7.500000000000000000 ) ) ;
#20437 = VERTEX_POINT ( 'NONE', #3050 ) ;
#20438 = CARTESIAN_POINT ( 'NONE',  ( -15.95292532278785913, -34.11873716947361856, 68.50000000000000000 ) ) ;
#20439 = ORIENTED_EDGE ( 'NONE', *, *, #5541, .T. ) ;
#20440 = CARTESIAN_POINT ( 'NONE',  ( 29.50000000000002132, 2.512390033608338236, -150.0833101980363722 ) ) ;
#20441 = PLANE ( 'NONE',  #9478 ) ;
#20442 = AXIS2_PLACEMENT_3D ( 'NONE', #12886, #9674, #14684 ) ;
#20443 = CARTESIAN_POINT ( 'NONE',  ( 0.000000000000000000, 52.39333383871510108, 13.79999999999999893 ) ) ;
#20444 = ORIENTED_EDGE ( 'NONE', *, *, #22050, .F. ) ;
#20445 = AXIS2_PLACEMENT_3D ( 'NONE', #18057, #19528, #2741 ) ;
#20446 = EDGE_LOOP ( 'NONE', ( #2183, #4034, #6357, #1402 ) ) ;
#20447 = VERTEX_POINT ( 'NONE', #1034 ) ;
#20448 = DIRECTION ( 'NONE',  ( -1.000000000000000000, 0.000000000000000000, 0.000000000000000000 ) ) ;
#20449 = DIRECTION ( 'NONE',  ( 0.000000000000000000, 1.000000000000000000, 0.000000000000000000 ) ) ;
#20450 = CIRCLE ( 'NONE', #18270, 0.3000000000000016542 ) ;
#20451 = CIRCLE ( 'NONE', #10443, 0.05000000000000143219 ) ;
#20452 = ORIENTED_EDGE ( 'NONE', *, *, #7152, .F. ) ;
#20453 = EDGE_CURVE ( 'NONE', #13600, #14227, #18372, .T. ) ;
#20454 = ORIENTED_EDGE ( 'NONE', *, *, #1284, .F. ) ;
#20455 = DIRECTION ( 'NONE',  ( 1.000000000000000000, 0.000000000000000000, 0.000000000000000000 ) ) ;
#20456 = MANIFOLD_SOLID_BREP ( 'Stock-MAS-696-1', #16326 ) ;
#20457 = ORIENTED_EDGE ( 'NONE', *, *, #15782, .T. ) ;
#20458 = DIRECTION ( 'NONE',  ( 0.000000000000000000, 0.000000000000000000, 1.000000000000000000 ) ) ;
#20459 = DIRECTION ( 'NONE',  ( 0.000000000000000000, 0.000000000000000000, 1.000000000000000000 ) ) ;
#20460 = FACE_OUTER_BOUND ( 'NONE', #18305, .T. ) ;
#20461 = DIRECTION ( 'NONE',  ( 3.052134192567367925E-16, 1.000000000000000000, 0.000000000000000000 ) ) ;
#20462 = ORIENTED_EDGE ( 'NONE', *, *, #226, .F. ) ;
#20463 = DIRECTION ( 'NONE',  ( 1.000000000000000000, -8.881784197001252323E-16, 0.000000000000000000 ) ) ;
#20464 = CARTESIAN_POINT ( 'NONE',  ( -1.774728116533986544, 42.31054587065082728, 39.80876104995653719 ) ) ;
#20465 = EDGE_CURVE ( 'NONE', #19660, #18731, #12, .T. ) ;
#20466 = AXIS2_PLACEMENT_3D ( 'NONE', #19251, #15653, #430 ) ;
#20467 = EDGE_CURVE ( 'NONE', #1975, #9891, #15373, .T. ) ;
#20468 = CIRCLE ( 'NONE', #6176, 0.05000000000000143219 ) ;
#20469 = EDGE_CURVE ( 'NONE', #6754, #16486, #18236, .T. ) ;
#20470 = DIRECTION ( 'NONE',  ( 1.000000000000000000, -0.000000000000000000, -0.000000000000000000 ) ) ;
#20471 = DIRECTION ( 'NONE',  ( 1.000000000000000000, -1.334402673828314029E-15, 0.000000000000000000 ) ) ;
#20472 = EDGE_LOOP ( 'NONE', ( #11606, #19932, #11551, #4335 ) ) ;
#20473 = DIRECTION ( 'NONE',  ( 1.000000000000000000, -0.000000000000000000, 6.123233995736764803E-17 ) ) ;
#20474 = EDGE_CURVE ( 'NONE', #3329, #10953, #2159, .T. ) ;
#20475 = DIRECTION ( 'NONE',  ( -0.000000000000000000, 1.000000000000000000, -0.000000000000000000 ) ) ;
#20476 = EDGE_LOOP ( 'NONE', ( #14829, #7311, #16349, #17167 ) ) ;
#20477 = DIRECTION ( 'NONE',  ( 1.000000000000000000, -2.832483164223420229E-16, 0.000000000000000000 ) ) ;
#20478 = CARTESIAN_POINT ( 'NONE',  ( -0.000000000000000000, -69.00000000000000000, 1.500000000000000000 ) ) ;
#20479 = EDGE_LOOP ( 'NONE', ( #13971, #15769, #14827, #1909 ) ) ;
#20480 = CARTESIAN_POINT ( 'NONE',  ( 1.724728116533979616, 43.26054587065083012, 53.76679706732590347 ) ) ;
#20481 = AXIS2_PLACEMENT_3D ( 'NONE', #21494, #11273, #16302 ) ;
#20482 = EDGE_CURVE ( 'NONE', #19361, #19672, #12151, .T. ) ;
#20483 = ORIENTED_EDGE ( 'NONE', *, *, #9474, .T. ) ;
#20484 = FACE_OUTER_BOUND ( 'NONE', #21850, .T. ) ;
#20485 = ORIENTED_EDGE ( 'NONE', *, *, #1135, .T. ) ;
#20486 = DIRECTION ( 'NONE',  ( -1.000000000000000000, 2.832483164223434527E-16, 0.000000000000000000 ) ) ;
#20487 = DIRECTION ( 'NONE',  ( -1.000000000000000000, 0.000000000000000000, 0.000000000000000000 ) ) ;
#20488 = CARTESIAN_POINT ( 'NONE',  ( -34.40000000000001279, -85.00000000000000000, 79.39999999999999147 ) ) ;
#20489 = DIRECTION ( 'NONE',  ( 0.000000000000000000, 0.000000000000000000, -1.000000000000000000 ) ) ;
#20490 = EDGE_CURVE ( 'NONE', #17432, #6971, #14311, .T. ) ;
#20491 = DIRECTION ( 'NONE',  ( -0.000000000000000000, 0.000000000000000000, -1.000000000000000000 ) ) ;
#20492 = DIRECTION ( 'NONE',  ( 0.000000000000000000, 1.000000000000000000, 0.000000000000000000 ) ) ;
#20493 = EDGE_CURVE ( 'NONE', #6037, #10046, #21483, .T. ) ;
#20494 = LINE ( 'NONE', #3, #5165 ) ;
#20495 = CARTESIAN_POINT ( 'NONE',  ( 14.96174975910705918, 51.76873716947361714, 13.79999999999999716 ) ) ;
#20496 = ORIENTED_EDGE ( 'NONE', *, *, #3830, .T. ) ;
#20497 = FACE_OUTER_BOUND ( 'NONE', #15095, .T. ) ;
#20498 = CARTESIAN_POINT ( 'NONE',  ( -23.37634868863050031, 45.32016349109721176, 13.74999999999999822 ) ) ;
#20499 = EDGE_LOOP ( 'NONE', ( #11994, #16952, #9866, #9476 ) ) ;
#20500 = ORIENTED_EDGE ( 'NONE', *, *, #7728, .T. ) ;
#20501 = DIRECTION ( 'NONE',  ( 0.000000000000000000, 0.000000000000000000, -1.000000000000000000 ) ) ;
#20502 = CARTESIAN_POINT ( 'NONE',  ( 0.000000000000000000, 0.000000000000000000, 0.000000000000000000 ) ) ;
#20503 = ORIENTED_EDGE ( 'NONE', *, *, #417, .T. ) ;
#20504 = FILL_AREA_STYLE ('',( #8648 ) ) ;
#20505 = ADVANCED_FACE ( 'NONE', ( #20172 ), #1818, .T. ) ;
#20506 = EDGE_LOOP ( 'NONE', ( #8840, #13845, #19163, #12876 ) ) ;
#20507 = EDGE_CURVE ( 'NONE', #8082, #21431, #15237, .T. ) ;
#20508 = ORIENTED_EDGE ( 'NONE', *, *, #17304, .T. ) ;
#20509 = CARTESIAN_POINT ( 'NONE',  ( -15.21174975910705207, -52.39333383871510108, 13.50000000000000000 ) ) ;
#20510 = DIRECTION ( 'NONE',  ( 0.000000000000000000, 1.000000000000000000, 0.000000000000000000 ) ) ;
#20511 = DIRECTION ( 'NONE',  ( -1.000000000000000000, 0.000000000000000000, 0.000000000000000000 ) ) ;
#20512 = EDGE_CURVE ( 'NONE', #16312, #573, #12861, .T. ) ;
#20513 = DIRECTION ( 'NONE',  ( 0.000000000000000000, 0.000000000000000000, 1.000000000000000000 ) ) ;
#20514 = DIRECTION ( 'NONE',  ( 0.000000000000000000, 0.000000000000000000, 1.000000000000000000 ) ) ;
#20515 = STYLED_ITEM ( 'NONE', ( #3516 ), #2184 ) ;
#20516 = DIRECTION ( 'NONE',  ( 1.000000000000000000, 0.000000000000000000, 0.000000000000000000 ) ) ;
#20517 = DIRECTION ( 'NONE',  ( -1.224646799147353207E-16, -0.000000000000000000, -1.000000000000000000 ) ) ;
#20518 = DIRECTION ( 'NONE',  ( -1.000000000000000000, 0.000000000000000000, 0.000000000000000000 ) ) ;
#20519 = ORIENTED_EDGE ( 'NONE', *, *, #5382, .F. ) ;
#20520 = VERTEX_POINT ( 'NONE', #4841 ) ;
#20521 = EDGE_LOOP ( 'NONE', ( #21900, #22125, #19643, #2680 ) ) ;
#20522 = DIRECTION ( 'NONE',  ( 0.2309407893631744979, -0.9729678061520400378, 0.000000000000000000 ) ) ;
#20523 = SURFACE_STYLE_USAGE ( .BOTH. , #19061 ) ;
#20524 = CARTESIAN_POINT ( 'NONE',  ( -15.21174975910705207, 41.81054587065082728, 68.25000000000000000 ) ) ;
#20525 = AXIS2_PLACEMENT_3D ( 'NONE', #2306, #5801, #17533 ) ;
#20526 = ORIENTED_EDGE ( 'NONE', *, *, #18443, .T. ) ;
#20527 = DIRECTION ( 'NONE',  ( 1.224646799147353207E-16, 0.000000000000000000, 1.000000000000000000 ) ) ;
#20528 = EDGE_CURVE ( 'NONE', #4986, #4038, #6113, .T. ) ;
#20529 = AXIS2_PLACEMENT_3D ( 'NONE', #11087, #19709, #16214 ) ;
#20530 = DIRECTION ( 'NONE',  ( 0.000000000000000000, 0.000000000000000000, 1.000000000000000000 ) ) ;
#20531 = DIRECTION ( 'NONE',  ( 1.000000000000000000, 0.000000000000000000, 0.000000000000000000 ) ) ;
#20532 = EDGE_CURVE ( 'NONE', #18590, #5820, #2515, .T. ) ;
#20533 = AXIS2_PLACEMENT_3D ( 'NONE', #57, #19998, #11470 ) ;
#20534 = DIRECTION ( 'NONE',  ( 1.788744114411106313E-17, 1.000000000000000000, 1.095289877103613968E-33 ) ) ;
#20535 = CARTESIAN_POINT ( 'NONE',  ( -8.641460742840918030, 33.43424481021354921, 68.00000000000000000 ) ) ;
#20536 = ORIENTED_EDGE ( 'NONE', *, *, #8938, .F. ) ;
#20537 = DIRECTION ( 'NONE',  ( 0.000000000000000000, 1.000000000000000000, 0.000000000000000000 ) ) ;
#20538 = CYLINDRICAL_SURFACE ( 'NONE', #674, 3.017785046117004377 ) ;
#20539 = CARTESIAN_POINT ( 'NONE',  ( 9.178906393579156386, 42.46645089659917716, 70.50000000000000000 ) ) ;
#20540 = DIRECTION ( 'NONE',  ( 0.000000000000000000, 0.000000000000000000, 1.000000000000000000 ) ) ;
#20541 = VERTEX_POINT ( 'NONE', #3172 ) ;
#20542 = DIRECTION ( 'NONE',  ( 0.000000000000000000, 1.000000000000000000, 0.000000000000000000 ) ) ;
#20543 = CARTESIAN_POINT ( 'NONE',  ( 33.19999999999999574, -84.70000000000001705, 78.79999999999999716 ) ) ;
#20544 = EDGE_LOOP ( 'NONE', ( #6306, #5390, #9531, #7294 ) ) ;
#20545 = DIRECTION ( 'NONE',  ( 0.000000000000000000, 0.000000000000000000, 1.000000000000000000 ) ) ;
#20546 = DIRECTION ( 'NONE',  ( 0.000000000000000000, -0.000000000000000000, 1.000000000000000000 ) ) ;
#20547 = FACE_OUTER_BOUND ( 'NONE', #1933, .T. ) ;
#20548 = ADVANCED_FACE ( 'NONE', ( #5182 ), #6767, .F. ) ;
#20549 = EDGE_LOOP ( 'NONE', ( #21578, #13001, #4411, #19095 ) ) ;
#20550 = ORIENTED_EDGE ( 'NONE', *, *, #3173, .T. ) ;
#20551 = AXIS2_PLACEMENT_3D ( 'NONE', #456, #15558, #8980 ) ;
#20552 = ORIENTED_EDGE ( 'NONE', *, *, #4482, .F. ) ;
#20553 = CARTESIAN_POINT ( 'NONE',  ( 23.32398829872514057, 7.118794219358020148E-15, 13.50000000000000000 ) ) ;
#20554 = PLANE ( 'NONE',  #2045 ) ;
#20555 = ADVANCED_FACE ( 'NONE', ( #20407 ), #15352, .T. ) ;
#20556 = B_SPLINE_CURVE_WITH_KNOTS ( 'NONE', 3,
 ( #9165, #21157, #2453, #7385, #20919, #15756, #5829, #8841 ),
 .UNSPECIFIED., .F., .F.,
 ( 4, 2, 2, 4 ),
 ( 0.000000000000000000, 0.0002326155127978793088, 0.0004652310255957586176, 0.0009304620511915139827 ),
 .UNSPECIFIED. ) ;
#20557 = VERTEX_POINT ( 'NONE', #10336 ) ;
#20558 = CARTESIAN_POINT ( 'NONE',  ( 3.127054932750481964, 32.11873716947361856, 42.50000000000000711 ) ) ;
#20559 = ORIENTED_EDGE ( 'NONE', *, *, #21300, .T. ) ;
#20560 = CARTESIAN_POINT ( 'NONE',  ( 1.774728116533979660, 42.31054587065082728, 53.66679706732590915 ) ) ;
#20561 = DIRECTION ( 'NONE',  ( -1.000000000000000000, -0.000000000000000000, -0.000000000000000000 ) ) ;
#20562 = AXIS2_PLACEMENT_3D ( 'NONE', #17860, #18070, #844 ) ;
#20563 = DIRECTION ( 'NONE',  ( -0.000000000000000000, 0.000000000000000000, -1.000000000000000000 ) ) ;
#20564 = VECTOR ( 'NONE', #20473, 1000.000000000000000 ) ;
#20565 = CARTESIAN_POINT ( 'NONE',  ( -33.20000000000001705, -84.70000000000001705, 78.79999999999999716 ) ) ;
#20566 = ORIENTED_EDGE ( 'NONE', *, *, #3683, .T. ) ;
#20567 = DIRECTION ( 'NONE',  ( 0.000000000000000000, 0.000000000000000000, -1.000000000000000000 ) ) ;
#20568 = DIRECTION ( 'NONE',  ( -0.000000000000000000, -0.000000000000000000, -1.000000000000000000 ) ) ;
#20569 = PLANE ( 'NONE',  #5158 ) ;
#20570 = PRODUCT_DEFINITION_SHAPE ( 'NONE', 'NONE',  #22166 ) ;
#20571 = DIRECTION ( 'NONE',  ( -1.000000000000000000, 0.000000000000000000, 1.445602896647331225E-15 ) ) ;
#20572 = ORIENTED_EDGE ( 'NONE', *, *, #19141, .T. ) ;
#20573 = CARTESIAN_POINT ( 'NONE',  ( 0.000000000000000000, 39.04634676501046187, 13.79999999999999893 ) ) ;
#20574 = EDGE_CURVE ( 'NONE', #3156, #20557, #13602, .T. ) ;
#20575 = DIRECTION ( 'NONE',  ( 0.000000000000000000, 1.000000000000000000, 0.000000000000000000 ) ) ;
#20576 = ORIENTED_EDGE ( 'NONE', *, *, #17467, .F. ) ;
#20577 = CIRCLE ( 'NONE', #14467, 0.04999999999999991257 ) ;
#20578 = FACE_OUTER_BOUND ( 'NONE', #15822, .T. ) ;
#20579 = CARTESIAN_POINT ( 'NONE',  ( 29.69597781366221767, 25.99124249474150972, 70.50000000000000000 ) ) ;
#20580 = CIRCLE ( 'NONE', #20922, 0.04999999999999991257 ) ;
#20581 = ORIENTED_EDGE ( 'NONE', *, *, #417, .F. ) ;
#20582 = VECTOR ( 'NONE', #16837, 1000.000000000000000 ) ;
#20583 = AXIS2_PLACEMENT_3D ( 'NONE', #18185, #7910, #14812 ) ;
#20584 = CARTESIAN_POINT ( 'NONE',  ( 1.724728116533979616, 42.36054587065083155, 43.75876104995654003 ) ) ;
#20585 = EDGE_CURVE ( 'NONE', #12515, #3217, #2896, .T. ) ;
#20586 = ADVANCED_FACE ( 'NONE', ( #10654 ), #5852, .F. ) ;
#20587 = ORIENTED_EDGE ( 'NONE', *, *, #3066, .F. ) ;
#20588 = DIRECTION ( 'NONE',  ( 0.000000000000000000, 0.000000000000000000, -1.000000000000000000 ) ) ;
#20589 = ORIENTED_EDGE ( 'NONE', *, *, #9673, .T. ) ;
#20590 = DIRECTION ( 'NONE',  ( 0.000000000000000000, 1.000000000000000000, 0.000000000000000000 ) ) ;
#20591 = TOROIDAL_SURFACE ( 'NONE', #2376, 0.5999999999999999778, 0.2999999999999999889 ) ;
#20592 = CARTESIAN_POINT ( 'NONE',  ( 31.44597781366222122, 56.94165929845684104, 70.50000000000000000 ) ) ;
#20593 = DIRECTION ( 'NONE',  ( 0.000000000000000000, 0.000000000000000000, -1.000000000000000000 ) ) ;
#20594 = MANIFOLD_SOLID_BREP ( 'Stock-MAS-696-1', #13821 ) ;
#20595 = CARTESIAN_POINT ( 'NONE',  ( -15.95292532278785913, 50.11873716947361856, 68.00000000000000000 ) ) ;
#20596 = AXIS2_PLACEMENT_3D ( 'NONE', #21726, #9300, #884 ) ;
#20597 = CONICAL_SURFACE ( 'NONE', #1271, 3077.683537175317724, 1.256637061435923464 ) ;
#20598 = EDGE_CURVE ( 'NONE', #17139, #17752, #19474, .T. ) ;
#20599 = DIRECTION ( 'NONE',  ( 0.000000000000000000, -0.000000000000000000, -1.000000000000000000 ) ) ;
#20600 = CARTESIAN_POINT ( 'NONE',  ( -14.96174975910705207, -51.76873716947361714, 13.79999999999999893 ) ) ;
#20601 = VERTEX_POINT ( 'NONE', #15883 ) ;
#20602 = PLANE ( 'NONE',  #12037 ) ;
#20603 = FACE_OUTER_BOUND ( 'NONE', #19415, .T. ) ;
#20604 = CARTESIAN_POINT ( 'NONE',  ( 1.724728116533979838, 43.26054587065083012, 53.66679706732590915 ) ) ;
#20605 = VECTOR ( 'NONE', #17796, 1000.000000000000000 ) ;
#20606 = CIRCLE ( 'NONE', #16650, 0.04999999999999991257 ) ;
#20607 = EDGE_LOOP ( 'NONE', ( #20365, #15172, #8725, #4552 ) ) ;
#20608 = AXIS2_PLACEMENT_3D ( 'NONE', #15328, #6516, #9968 ) ;
#20609 = EDGE_LOOP ( 'NONE', ( #5735, #18408, #19038, #123 ) ) ;
#20610 = CARTESIAN_POINT ( 'NONE',  ( 1.724728116533979616, 42.31054587065082728, 35.75876104995654003 ) ) ;
#20611 = DIRECTION ( 'NONE',  ( 0.000000000000000000, 0.000000000000000000, 1.000000000000000000 ) ) ;
#20612 = EDGE_CURVE ( 'NONE', #20854, #11511, #16078, .T. ) ;
#20613 = ORIENTED_EDGE ( 'NONE', *, *, #825, .T. ) ;
#20614 = EDGE_CURVE ( 'NONE', #12641, #6442, #14658, .T. ) ;
#20615 = VECTOR ( 'NONE', #16113, 1000.000000000000000 ) ;
#20616 = ADVANCED_FACE ( 'NONE', ( #15779 ), #9191, .T. ) ;
#20617 = EDGE_LOOP ( 'NONE', ( #14153, #10587, #20910, #13551 ) ) ;
#20618 = ORIENTED_EDGE ( 'NONE', *, *, #19801, .F. ) ;
#20619 = DIRECTION ( 'NONE',  ( 8.673617379884034239E-17, 0.000000000000000000, -1.000000000000000000 ) ) ;
#20620 = DIRECTION ( 'NONE',  ( 1.000000000000000000, 3.052134192567374827E-16, 0.000000000000000000 ) ) ;
#20621 = CIRCLE ( 'NONE', #12722, 0.2500000000000002220 ) ;
#20622 = AXIS2_PLACEMENT_3D ( 'NONE', #19434, #5905, #16407 ) ;
#20623 = CARTESIAN_POINT ( 'NONE',  ( -21.92816239687475743, 42.46645089659918426, 13.74999999999999822 ) ) ;
#20624 = CIRCLE ( 'NONE', #2377, 0.05000000000000143219 ) ;
#20625 =( NAMED_UNIT ( * ) PLANE_ANGLE_UNIT ( ) SI_UNIT ( $, .RADIAN. ) );
#20626 = FACE_OUTER_BOUND ( 'NONE', #7585, .T. ) ;
#20627 = DIRECTION ( 'NONE',  ( -1.000000000000000000, 0.000000000000000000, 0.000000000000000000 ) ) ;
#20628 = LINE ( 'NONE', #353, #15176 ) ;
#20629 = DIRECTION ( 'NONE',  ( 0.000000000000000000, 0.000000000000000000, 1.000000000000000000 ) ) ;
#20630 = AXIS2_PLACEMENT_3D ( 'NONE', #3425, #8697, #13702 ) ;
#20631 = ADVANCED_FACE ( 'NONE', ( #2025 ), #20733, .T. ) ;
#20632 = DIRECTION ( 'NONE',  ( 0.000000000000000000, 0.000000000000000000, 1.000000000000000000 ) ) ;
#20633 = EDGE_LOOP ( 'NONE', ( #21415, #13727, #18494, #15244 ) ) ;
#20634 = ORIENTED_EDGE ( 'NONE', *, *, #12616, .T. ) ;
#20635 = CARTESIAN_POINT ( 'NONE',  ( 30.49999999999999645, -84.70000000000001705, 1.200000000000003064 ) ) ;
#20636 =( NAMED_UNIT ( * ) SI_UNIT ( $, .STERADIAN. ) SOLID_ANGLE_UNIT ( ) );
#20637 = CARTESIAN_POINT ( 'NONE',  ( -30.49999999999998934, 69.70000000000001705, 1.199999999999999734 ) ) ;
#20638 = ORIENTED_EDGE ( 'NONE', *, *, #14084, .T. ) ;
#20639 = VECTOR ( 'NONE', #15260, 1000.000000000000000 ) ;
#20640 = CLOSED_SHELL ( 'NONE', ( #10439, #8256, #10880, #3051, #20913, #692, #18795, #14393, #11626, #21035, #13294, #5279, #10278, #5575, #13779, #13266, #19669, #3539, #9794, #9889, #20978, #15838, #15570, #19715, #5725, #7629, #9915, #12851, #144, #17788, #14577, #12268, #15343, #16554, #6906, #15238, #19780, #18967, #21749, #7880, #13313, #10334, #8393, #5460, #1954, #8835, #5509, #6538, #14173, #17646, #331, #11999, #3793, #3931, #7187, #19407, #3373, #9004, #11611, #3112, #10353, #17694, #21946, #7596, #1546, #12949, #7574, #17990, #18386, #2323, #11718, #8751, #8594, #21621, #16541, #12712, #8689, #20586, #13711, #4056, #2535, #16463, #3587, #12048, #17470, #13866, #21072, #2133, #2026, #11019, #683, #5384, #16931, #11722, #5428, #16250, #20082, #7291, #14648, #7244, #3919, #19659, #21977, #20146, #11868, #5177, #4993, #11400, #6854, #5781, #10418, #1318, #15633, #21339, #4123, #20725, #8408, #16075, #8445, #13501, #468, #17804, #5195, #13897, #16999, #8676, #19243, #20505, #8281, #11823, #16543, #19785, #7754, #1415, #1519, #10296, #6059, #15900, #17455, #3968, #11405, #7647, #14171, #19692, #11735, #13587, #10596, #15544, #10304, #5410, #4789, #15571, #3438, #6728, #7749, #3402, #4497, #5301, #19856, #4917, #8505, #4819, #10197, #2875, #20193, #6280, #10191, #18365, #6937, #19409, #13813, #20103, #2326, #8161, #7957, #1828, #4341, #6449, #1029, #804, #3810, #21834, #13465, #4324, #10553 ) ) ;
#20641 = CIRCLE ( 'NONE', #13463, 6.800000000000000711 ) ;
#20642 = TOROIDAL_SURFACE ( 'NONE', #4544, 0.05000000000000000278, 0.05000000000000000278 ) ;
#20643 = EDGE_CURVE ( 'NONE', #445, #3156, #8869, .T. ) ;
#20644 = CIRCLE ( 'NONE', #6355, 0.2499999999999985012 ) ;
#20645 = CARTESIAN_POINT ( 'NONE',  ( -15.21174975910705207, -52.11873716947361856, 68.00000000000000000 ) ) ;
#20646 = AXIS2_PLACEMENT_3D ( 'NONE', #5190, #8330, #13777 ) ;
#20647 = FACE_OUTER_BOUND ( 'NONE', #2902, .T. ) ;
#20648 = DIRECTION ( 'NONE',  ( 1.000000000000000000, 0.000000000000000000, -0.000000000000000000 ) ) ;
#20649 = ORIENTED_EDGE ( 'NONE', *, *, #18596, .T. ) ;
#20650 = DIRECTION ( 'NONE',  ( -0.000000000000000000, 0.000000000000000000, 1.000000000000000000 ) ) ;
#20651 = CARTESIAN_POINT ( 'NONE',  ( 1.724728116533979616, 42.36054587065083155, 43.70876104995653577 ) ) ;
#20652 = CARTESIAN_POINT ( 'NONE',  ( 1.724728116533979838, 43.26054587065083012, 33.66679706732590915 ) ) ;
#20653 = FACE_OUTER_BOUND ( 'NONE', #11967, .T. ) ;
#20654 = CYLINDRICAL_SURFACE ( 'NONE', #14683, 0.2500000000000002220 ) ;
#20655 = AXIS2_PLACEMENT_3D ( 'NONE', #6822, #12143, #15173 ) ;
#20656 = CIRCLE ( 'NONE', #5996, 0.2500000000000002220 ) ;
#20657 = CARTESIAN_POINT ( 'NONE',  ( 29.17540678000427690, 63.74634676501045050, 7.500000000000000000 ) ) ;
#20658 = ADVANCED_FACE ( 'NONE', ( #17583 ), #15554, .T. ) ;
#20659 = CARTESIAN_POINT ( 'NONE',  ( 15.21174975910705918, 41.81054587065082728, 13.75000000000000000 ) ) ;
#20660 = DIRECTION ( 'NONE',  ( -0.000000000000000000, -0.000000000000000000, 1.000000000000000000 ) ) ;
#20661 = CIRCLE ( 'NONE', #9919, 2.000000000000001776 ) ;
#20662 = DIRECTION ( 'NONE',  ( 0.000000000000000000, 0.000000000000000000, -1.000000000000000000 ) ) ;
#20663 = EDGE_CURVE ( 'NONE', #5533, #15579, #365, .T. ) ;
#20664 = ORIENTED_EDGE ( 'NONE', *, *, #19303, .F. ) ;
#20665 = VERTEX_POINT ( 'NONE', #17679 ) ;
#20666 = AXIS2_PLACEMENT_3D ( 'NONE', #7312, #13896, #12643 ) ;
#20667 = ORIENTED_EDGE ( 'NONE', *, *, #17617, .F. ) ;
#20668 = DIRECTION ( 'NONE',  ( -1.000000000000000000, 0.000000000000000000, 0.000000000000000000 ) ) ;
#20669 = CARTESIAN_POINT ( 'NONE',  ( 31.50000000000002132, -72.00000000000001421, 3.500000000000000000 ) ) ;
#20670 = VECTOR ( 'NONE', #9017, 1000.000000000000000 ) ;
#20671 = CARTESIAN_POINT ( 'NONE',  ( -14.96174975910705207, 42.31054587065082728, 13.75000000000000000 ) ) ;
#20672 = EDGE_LOOP ( 'NONE', ( #945, #3034, #16008, #68, #3484, #3774, #8824, #3941 ) ) ;
#20673 = DIRECTION ( 'NONE',  ( 0.000000000000000000, 0.000000000000000000, 1.000000000000000000 ) ) ;
#20674 = AXIS2_PLACEMENT_3D ( 'NONE', #6998, #17165, #4867 ) ;
#20675 = VECTOR ( 'NONE', #5586, 1000.000000000000000 ) ;
#20676 = ORIENTED_EDGE ( 'NONE', *, *, #8247, .F. ) ;
#20677 = CARTESIAN_POINT ( 'NONE',  ( -25.37540678000427263, -63.74634676501045050, 3.500000000000000000 ) ) ;
#20678 = DIRECTION ( 'NONE',  ( -1.327594496921025717E-16, -1.000000000000000000, 1.625834351219974904E-32 ) ) ;
#20679 = AXIS2_PLACEMENT_3D ( 'NONE', #6047, #9275, #17984 ) ;
#20680 = EDGE_CURVE ( 'NONE', #14823, #8599, #3245, .T. ) ;
#20681 = LINE ( 'NONE', #20788, #14645 ) ;
#20682 = VECTOR ( 'NONE', #3844, 1000.000000000000000 ) ;
#20683 = LINE ( 'NONE', #3225, #6899 ) ;
#20684 = VERTEX_POINT ( 'NONE', #19378 ) ;
#20685 = CARTESIAN_POINT ( 'NONE',  ( 23.02398829872490182, 2.928742984578568631, 13.54178985689097736 ) ) ;
#20686 = CIRCLE ( 'NONE', #16358, 0.04999999999999991257 ) ;
#20687 = CARTESIAN_POINT ( 'NONE',  ( 14.96174975910707161, 51.61873716947361856, 68.00000000000000000 ) ) ;
#20688 = CARTESIAN_POINT ( 'NONE',  ( -3.127054932750481964, -32.61873716947361856, 68.00000000000000000 ) ) ;
#20689 = DIRECTION ( 'NONE',  ( 1.788744114411106313E-17, 1.000000000000000000, 1.095289877103613968E-33 ) ) ;
#20690 = ORIENTED_EDGE ( 'NONE', *, *, #17702, .T. ) ;
#20691 = PLANE ( 'NONE',  #21280 ) ;
#20692 = EDGE_CURVE ( 'NONE', #8060, #15052, #3613, .T. ) ;
#20693 = ORIENTED_EDGE ( 'NONE', *, *, #9991, .F. ) ;
#20694 = CARTESIAN_POINT ( 'NONE',  ( -34.40000000000001279, 84.70000000000001705, 79.70000000000000284 ) ) ;
#20695 = VECTOR ( 'NONE', #18601, 1000.000000000000000 ) ;
#20696 = ORIENTED_EDGE ( 'NONE', *, *, #12072, .T. ) ;
#20697 = CARTESIAN_POINT ( 'NONE',  ( 1.824728116533979261, 42.36054587065083155, 47.70876104995654288 ) ) ;
#20698 = DIRECTION ( 'NONE',  ( -1.000000000000000000, 0.000000000000000000, -0.000000000000000000 ) ) ;
#20699 = VERTEX_POINT ( 'NONE', #21620 ) ;
#20700 = AXIS2_PLACEMENT_3D ( 'NONE', #4582, #21495, #768 ) ;
#20701 = ORIENTED_EDGE ( 'NONE', *, *, #3909, .F. ) ;
#20702 = EDGE_CURVE ( 'NONE', #16055, #7987, #21128, .T. ) ;
#20703 = EDGE_LOOP ( 'NONE', ( #4133, #2644, #5355, #21471 ) ) ;
#20704 = CARTESIAN_POINT ( 'NONE',  ( 18.22752199202934520, 38.74634676501045760, 13.79999999999999893 ) ) ;
#20705 = DIRECTION ( 'NONE',  ( -0.000000000000000000, -0.000000000000000000, -1.000000000000000000 ) ) ;
#20706 = FACE_OUTER_BOUND ( 'NONE', #15456, .T. ) ;
#20707 = AXIS2_PLACEMENT_3D ( 'NONE', #21670, #8237, #13476 ) ;
#20708 = CARTESIAN_POINT ( 'NONE',  ( 29.48703555828264911, 2.527994776753299533, 0.2022843821483596705 ) ) ;
#20709 = EDGE_CURVE ( 'NONE', #20437, #8649, #4481, .T. ) ;
#20710 = CIRCLE ( 'NONE', #11050, 0.1000000000000028644 ) ;
#20711 = FACE_OUTER_BOUND ( 'NONE', #16586, .T. ) ;
#20712 = EDGE_CURVE ( 'NONE', #11228, #12849, #17532, .T. ) ;
#20713 = LINE ( 'NONE', #5389, #11156 ) ;
#20714 = EDGE_LOOP ( 'NONE', ( #1811, #19610, #21532 ) ) ;
#20715 = DIRECTION ( 'NONE',  ( 0.000000000000000000, 0.000000000000000000, 1.000000000000000000 ) ) ;
#20716 = FACE_OUTER_BOUND ( 'NONE', #12208, .T. ) ;
#20717 = ORIENTED_EDGE ( 'NONE', *, *, #6958, .F. ) ;
#20718 = VERTEX_POINT ( 'NONE', #16108 ) ;
#20719 = CARTESIAN_POINT ( 'NONE',  ( 0.000000000000000000, 43.31054587065082728, 16.00000000000000000 ) ) ;
#20720 = APPLICATION_PROTOCOL_DEFINITION ( 'draft international standard', 'automotive_design', 1998, #19880 ) ;
#20721 = AXIS2_PLACEMENT_3D ( 'NONE', #7832, #859, #4120 ) ;
#20722 = ORIENTED_EDGE ( 'NONE', *, *, #4496, .F. ) ;
#20723 = PRESENTATION_LAYER_ASSIGNMENT (  '', '', ( #338 ) ) ;
#20724 = CIRCLE ( 'NONE', #19279, 0.9652499999999990532 ) ;
#20725 = ADVANCED_FACE ( 'NONE', ( #4713 ), #13942, .T. ) ;
#20726 = CARTESIAN_POINT ( 'NONE',  ( 23.02398829872514341, -2.211005166398812616, 13.19999999999999041 ) ) ;
#20727 = VERTEX_POINT ( 'NONE', #9303 ) ;
#20728 = ORIENTED_EDGE ( 'NONE', *, *, #5563, .T. ) ;
#20729 = CARTESIAN_POINT ( 'NONE',  ( -31.44597781366221412, 27.99124249474150972, 68.50000000000000000 ) ) ;
#20730 = LINE ( 'NONE', #12294, #1990 ) ;
#20731 = DIRECTION ( 'NONE',  ( -1.000000000000000000, 0.000000000000000000, 0.000000000000000000 ) ) ;
#20732 = CARTESIAN_POINT ( 'NONE',  ( 23.02398829872514341, 2.333099608346429044, 13.47123417368288223 ) ) ;
#20733 = CYLINDRICAL_SURFACE ( 'NONE', #17874, 0.2500000000000002220 ) ;
#20734 =( REPRESENTATION_RELATIONSHIP ('NONE','NONE', #561, #6277 ) REPRESENTATION_RELATIONSHIP_WITH_TRANSFORMATION ( #9631 )SHAPE_REPRESENTATION_RELATIONSHIP( ) );
#20735 = EDGE_CURVE ( 'NONE', #18586, #22148, #11457, .T. ) ;
#20736 = AXIS2_PLACEMENT_3D ( 'NONE', #20781, #12242, #17728 ) ;
#20737 =( GEOMETRIC_REPRESENTATION_CONTEXT ( 3 ) GLOBAL_UNCERTAINTY_ASSIGNED_CONTEXT ( ( #13097 ) ) GLOBAL_UNIT_ASSIGNED_CONTEXT ( ( #21644, #1368, #9775 ) ) REPRESENTATION_CONTEXT ( 'NONE', 'WORKASPACE' ) );
#20738 = CARTESIAN_POINT ( 'NONE',  ( -23.02398829872513986, 2.211005166398795740, 13.19999999999999041 ) ) ;
#20739 = EDGE_CURVE ( 'NONE', #7598, #6237, #6074, .T. ) ;
#20740 = DIRECTION ( 'NONE',  ( 0.000000000000000000, 0.000000000000000000, 1.000000000000000000 ) ) ;
#20741 = CARTESIAN_POINT ( 'NONE',  ( -6.728906393579160650, 43.00645089659919762, 70.88527860057354246 ) ) ;
#20742 = DIRECTION ( 'NONE',  ( 0.000000000000000000, 0.000000000000000000, 1.000000000000000000 ) ) ;
#20743 = ADVANCED_FACE ( 'NONE', ( #7967 ), #19708, .F. ) ;
#20744 = CARTESIAN_POINT ( 'NONE',  ( -21.92816239687475743, 42.46645089659918426, 68.25000000000000000 ) ) ;
#20745 = CARTESIAN_POINT ( 'NONE',  ( -6.678906393579157275, 42.46645089659918426, 67.85468508031152624 ) ) ;
#20746 = ORIENTED_EDGE ( 'NONE', *, *, #5282, .F. ) ;
#20747 = ORIENTED_EDGE ( 'NONE', *, *, #14856, .T. ) ;
#20748 = DIRECTION ( 'NONE',  ( 1.000000000000000000, 0.000000000000000000, 0.000000000000000000 ) ) ;
#20749 = SURFACE_STYLE_FILL_AREA ( #13899 ) ;
#20750 = DIRECTION ( 'NONE',  ( -1.000000000000000000, 0.000000000000000000, 0.000000000000000000 ) ) ;
#20751 = VERTEX_POINT ( 'NONE', #2923 ) ;
#20752 = CARTESIAN_POINT ( 'NONE',  ( -14.96174975910705207, 32.10873716947361345, 13.05380965755523448 ) ) ;
#20753 = AXIS2_PLACEMENT_3D ( 'NONE', #10969, #2583, #3632 ) ;
#20754 = EDGE_CURVE ( 'NONE', #9603, #8176, #14769, .T. ) ;
#20755 = VECTOR ( 'NONE', #15675, 1000.000000000000000 ) ;
#20756 = LINE ( 'NONE', #17263, #16308 ) ;
#20757 = CYLINDRICAL_SURFACE ( 'NONE', #21667, 1.999999999999991340 ) ;
#20758 = EDGE_LOOP ( 'NONE', ( #3163, #8786, #1383, #8968 ) ) ;
#20759 = CARTESIAN_POINT ( 'NONE',  ( -31.63662752439705272, 0.000000000000000000, 1.500000000000001332 ) ) ;
#20760 = CARTESIAN_POINT ( 'NONE',  ( -1.724728116533986721, 43.31054587065082728, 49.66679706732590915 ) ) ;
#20761 = CARTESIAN_POINT ( 'NONE',  ( -14.96174975910705207, 51.61873716947361856, 13.75000000000000000 ) ) ;
#20762 = ADVANCED_FACE ( 'NONE', ( #18012 ), #19326, .T. ) ;
#20763 = CARTESIAN_POINT ( 'NONE',  ( 0.000000000000000000, 50.00000000000000000, 0.000000000000000000 ) ) ;
#20764 = CARTESIAN_POINT ( 'NONE',  ( 34.69999999999998863, 84.70000000000001705, 79.39999999999999147 ) ) ;
#20765 = CARTESIAN_POINT ( 'NONE',  ( 33.19999999999999574, -84.70000000000001705, 1.799999999999996048 ) ) ;
#20766 = EDGE_CURVE ( 'NONE', #9450, #1486, #12859, .T. ) ;
#20767 = PLANE ( 'NONE',  #20078 ) ;
#20768 = AXIS2_PLACEMENT_3D ( 'NONE', #14426, #7738, #14539 ) ;
#20769 = CARTESIAN_POINT ( 'NONE',  ( 33.79999999999999716, -85.00000000000000000, 1.799999999999996048 ) ) ;
#20770 = DIRECTION ( 'NONE',  ( 0.000000000000000000, 0.000000000000000000, 1.000000000000000000 ) ) ;
#20771 = ORIENTED_EDGE ( 'NONE', *, *, #21612, .F. ) ;
#20772 = EDGE_LOOP ( 'NONE', ( #1236, #9867, #11804, #14116 ) ) ;
#20773 = ORIENTED_EDGE ( 'NONE', *, *, #14513, .T. ) ;
#20774 = DIRECTION ( 'NONE',  ( 0.000000000000000000, 1.000000000000000000, 0.000000000000000000 ) ) ;
#20775 = DIRECTION ( 'NONE',  ( -1.224646799147353207E-16, 0.000000000000000000, -1.000000000000000000 ) ) ;
#20776 = DIRECTION ( 'NONE',  ( -1.000000000000000000, 0.000000000000000000, 0.000000000000000000 ) ) ;
#20777 = DIRECTION ( 'NONE',  ( 1.000000000000000000, -0.000000000000000000, 0.000000000000000000 ) ) ;
#20778 = AXIS2_PLACEMENT_3D ( 'NONE', #21675, #16504, #8131 ) ;
#20779 = CIRCLE ( 'NONE', #759, 0.05000000000000143219 ) ;
#20780 = ORIENTED_EDGE ( 'NONE', *, *, #16207, .F. ) ;
#20781 = CARTESIAN_POINT ( 'NONE',  ( 25.37540678000429040, -36.74634676501047181, 42.50000000000000000 ) ) ;
#20782 = EDGE_CURVE ( 'NONE', #1252, #9049, #16450, .T. ) ;
#20783 = VERTEX_POINT ( 'NONE', #17799 ) ;
#20784 = CARTESIAN_POINT ( 'NONE',  ( -28.86382559268571057, -6.505889654322387194, 13.29319881794719294 ) ) ;
#20785 = VECTOR ( 'NONE', #283, 1000.000000000000000 ) ;
#20786 = EDGE_CURVE ( 'NONE', #9883, #17139, #6855, .T. ) ;
#20787 = CARTESIAN_POINT ( 'NONE',  ( 1.724728116533979616, 42.36054587065083155, 27.70876104995653577 ) ) ;
#20788 = CARTESIAN_POINT ( 'NONE',  ( -8.638906393579159015, 40.01645089659919563, 70.88527860057354246 ) ) ;
#20789 = CARTESIAN_POINT ( 'NONE',  ( 28.87540678000427619, -63.74634676501045050, 7.799999999999999822 ) ) ;
#20790 = ORIENTED_EDGE ( 'NONE', *, *, #2679, .T. ) ;
#20791 = CARTESIAN_POINT ( 'NONE',  ( 23.02398829872536368, 2.681050038336382446, 13.50121499737447728 ) ) ;
#20792 = DIRECTION ( 'NONE',  ( -1.000000000000000000, -0.000000000000000000, 2.388292521039847891E-16 ) ) ;
#20793 = VECTOR ( 'NONE', #19734, 1000.000000000000000 ) ;
#20794 = CARTESIAN_POINT ( 'NONE',  ( 14.71174975910705740, 52.11873716947361856, 14.00000000000000000 ) ) ;
#20795 = DIRECTION ( 'NONE',  ( -1.000000000000000000, 0.000000000000000000, 0.000000000000000000 ) ) ;
#20796 = ORIENTED_EDGE ( 'NONE', *, *, #586, .F. ) ;
#20797 = PLANE ( 'NONE',  #20923 ) ;
#20798 = AXIS2_PLACEMENT_3D ( 'NONE', #15968, #14184, #12173 ) ;
#20799 = AXIS2_PLACEMENT_3D ( 'NONE', #4508, #2953, #9886 ) ;
#20800 = ORIENTED_EDGE ( 'NONE', *, *, #3831, .T. ) ;
#20801 = DIRECTION ( 'NONE',  ( -1.000000000000000000, 0.000000000000000000, 0.000000000000000000 ) ) ;
#20802 = VECTOR ( 'NONE', #10545, 1000.000000000000000 ) ;
#20803 = DIRECTION ( 'NONE',  ( 0.000000000000000000, 0.000000000000000000, -1.000000000000000000 ) ) ;
#20804 = VERTEX_POINT ( 'NONE', #6287 ) ;
#20805 = ORIENTED_EDGE ( 'NONE', *, *, #19155, .T. ) ;
#20806 = DIRECTION ( 'NONE',  ( -1.000000000000000000, 0.000000000000000000, 0.000000000000000000 ) ) ;
#20807 = CARTESIAN_POINT ( 'NONE',  ( 29.13662752439705272, 0.000000000000000000, 7.500000000000000000 ) ) ;
#20808 = ORIENTED_EDGE ( 'NONE', *, *, #12383, .T. ) ;
#20809 = ORIENTED_EDGE ( 'NONE', *, *, #16724, .T. ) ;
#20810 = VECTOR ( 'NONE', #17295, 1000.000000000000000 ) ;
#20811 = CIRCLE ( 'NONE', #16865, 0.5000000000000004441 ) ;
#20812 = EDGE_LOOP ( 'NONE', ( #2749, #1708, #9958, #2406 ) ) ;
#20813 = CARTESIAN_POINT ( 'NONE',  ( -15.95292532278785913, 52.10286008774954780, 13.87499999999999822 ) ) ;
#20814 = VECTOR ( 'NONE', #5721, 1000.000000000000000 ) ;
#20815 = EDGE_CURVE ( 'NONE', #17848, #9870, #12165, .T. ) ;
#20816 = PLANE ( 'NONE',  #15770 ) ;
#20817 = CYLINDRICAL_SURFACE ( 'NONE', #18501, 0.2999999999999999334 ) ;
#20818 = CARTESIAN_POINT ( 'NONE',  ( 0.000000000000000000, 43.26054587065083012, 31.75876104995653648 ) ) ;
#20819 = PRODUCT_DEFINITION_CONTEXT ( 'detailed design', #6598, 'design' ) ;
#20820 = ORIENTED_EDGE ( 'NONE', *, *, #3325, .T. ) ;
#20821 = DIRECTION ( 'NONE',  ( 0.000000000000000000, 0.000000000000000000, 1.000000000000000000 ) ) ;
#20822 = DIRECTION ( 'NONE',  ( 1.000000000000000000, 0.000000000000000000, 0.000000000000000000 ) ) ;
#20823 = CARTESIAN_POINT ( 'NONE',  ( -30.79999999999999361, -84.70000000000001705, 1.200000000000000622 ) ) ;
#20824 = ORIENTED_EDGE ( 'NONE', *, *, #6283, .F. ) ;
#20825 = DIRECTION ( 'NONE',  ( 0.000000000000000000, 0.000000000000000000, 1.000000000000000000 ) ) ;
#20826 = LINE ( 'NONE', #12079, #11324 ) ;
#20827 = VECTOR ( 'NONE', #6575, 1000.000000000000000 ) ;
#20828 = EDGE_CURVE ( 'NONE', #17812, #8454, #2687, .T. ) ;
#20829 = ORIENTED_EDGE ( 'NONE', *, *, #765, .F. ) ;
#20830 = ORIENTED_EDGE ( 'NONE', *, *, #18814, .F. ) ;
#20831 = DIRECTION ( 'NONE',  ( -1.000000000000000000, 0.000000000000000000, -0.000000000000000000 ) ) ;
#20832 = DIRECTION ( 'NONE',  ( 1.000000000000000000, 0.000000000000000000, 0.000000000000000000 ) ) ;
#20833 = ORIENTED_EDGE ( 'NONE', *, *, #18269, .T. ) ;
#20834 = EDGE_LOOP ( 'NONE', ( #10133, #6627, #13285, #8017 ) ) ;
#20835 = ADVANCED_FACE ( 'NONE', ( #16330 ), #9643, .F. ) ;
#20836 = ADVANCED_FACE ( 'NONE', ( #16550 ), #18128, .T. ) ;
#20837 = CARTESIAN_POINT ( 'NONE',  ( 29.69597781366221767, 56.94165929845684104, 70.25000000000000000 ) ) ;
#20838 = ORIENTED_EDGE ( 'NONE', *, *, #11414, .F. ) ;
#20839 = EDGE_LOOP ( 'NONE', ( #20613, #17399, #8327, #18197 ) ) ;
#20840 = DIRECTION ( 'NONE',  ( 1.000000000000000000, 0.000000000000000000, 0.000000000000000000 ) ) ;
#20841 = CYLINDRICAL_SURFACE ( 'NONE', #15561, 0.2999999999999999334 ) ;
#20842 = DIRECTION ( 'NONE',  ( 1.000000000000000000, 0.000000000000000000, 0.000000000000000000 ) ) ;
#20843 = FILL_AREA_STYLE ('',( #19272 ) ) ;
#20844 = DIRECTION ( 'NONE',  ( 0.000000000000000000, 0.000000000000000000, 1.000000000000000000 ) ) ;
#20845 = DIRECTION ( 'NONE',  ( 0.000000000000000000, 0.000000000000000000, -1.000000000000000000 ) ) ;
#20846 = CARTESIAN_POINT ( 'NONE',  ( -29.37540678000427619, 6.000000000000000000, 7.200000000000000178 ) ) ;
#20847 = DIRECTION ( 'NONE',  ( 0.000000000000000000, 0.000000000000000000, 1.000000000000000000 ) ) ;
#20848 = EDGE_CURVE ( 'NONE', #15046, #21877, #3253, .T. ) ;
#20849 = CARTESIAN_POINT ( 'NONE',  ( -14.96174975910705207, -51.76873716947361714, 13.79999999999999716 ) ) ;
#20850 = ORIENTED_EDGE ( 'NONE', *, *, #21069, .T. ) ;
#20851 = ORIENTED_EDGE ( 'NONE', *, *, #13103, .F. ) ;
#20852 = DIRECTION ( 'NONE',  ( -0.000000000000000000, -0.000000000000000000, -1.000000000000000000 ) ) ;
#20853 = DIRECTION ( 'NONE',  ( 0.000000000000000000, -1.000000000000000000, 0.000000000000000000 ) ) ;
#20854 = VERTEX_POINT ( 'NONE', #13541 ) ;
#20855 = EDGE_LOOP ( 'NONE', ( #21963, #282, #12404, #14312 ) ) ;
#20856 = EDGE_CURVE ( 'NONE', #21585, #13976, #749, .T. ) ;
#20857 = EDGE_CURVE ( 'NONE', #16560, #19513, #21497, .T. ) ;
#20858 = ADVANCED_FACE ( 'NONE', ( #16781 ), #3026, .F. ) ;
#20859 = EDGE_CURVE ( 'NONE', #21689, #15362, #17548, .T. ) ;
#20860 = CARTESIAN_POINT ( 'NONE',  ( -31.69597781366222122, 56.94165929845684815, 70.25000000000000000 ) ) ;
#20861 = CARTESIAN_POINT ( 'NONE',  ( 33.19999999999999574, -85.00000000000000000, 1.799999999999996048 ) ) ;
#20862 = ORIENTED_EDGE ( 'NONE', *, *, #21397, .F. ) ;
#20863 = DIRECTION ( 'NONE',  ( -1.000000000000000000, 1.094601647044990554E-16, -0.000000000000000000 ) ) ;
#20864 = DIRECTION ( 'NONE',  ( 0.000000000000000000, 0.000000000000000000, -1.000000000000000000 ) ) ;
#20865 = CARTESIAN_POINT ( 'NONE',  ( -27.37540678000428684, -36.74634676501047181, 13.79999999999999893 ) ) ;
#20866 = DIRECTION ( 'NONE',  ( -1.000000000000000000, 0.000000000000000000, 0.000000000000000000 ) ) ;
#20867 = CARTESIAN_POINT ( 'NONE',  ( 25.37540678000427263, 63.74634676501045050, 13.19999999999999929 ) ) ;
#20868 = CARTESIAN_POINT ( 'NONE',  ( 1.724728116533979616, 43.26054587065083012, 43.70876104995653577 ) ) ;
#20869 = FACE_OUTER_BOUND ( 'NONE', #10829, .T. ) ;
#20870 = EDGE_CURVE ( 'NONE', #13878, #10557, #1555, .T. ) ;
#20871 = ORIENTED_EDGE ( 'NONE', *, *, #3663, .T. ) ;
#20872 = DIRECTION ( 'NONE',  ( -0.000000000000000000, 0.000000000000000000, -1.000000000000000000 ) ) ;
#20873 = FACE_OUTER_BOUND ( 'NONE', #3873, .T. ) ;
#20874 = CARTESIAN_POINT ( 'NONE',  ( 29.50000000000001421, -69.00000000000000000, 0.1242640687119233311 ) ) ;
#20875 = VERTEX_POINT ( 'NONE', #9856 ) ;
#20876 = ORIENTED_EDGE ( 'NONE', *, *, #14595, .T. ) ;
#20877 = EDGE_LOOP ( 'NONE', ( #18720, #18140, #7662, #13218 ) ) ;
#20878 = CARTESIAN_POINT ( 'NONE',  ( 1.774728116533979438, 42.36054587065083155, 39.70876104995653577 ) ) ;
#20879 = DIRECTION ( 'NONE',  ( 0.000000000000000000, 0.000000000000000000, 1.000000000000000000 ) ) ;
#20880 = CARTESIAN_POINT ( 'NONE',  ( -34.70000000000000284, 84.70000000000001705, 0.6000000000000033085 ) ) ;
#20881 = EDGE_LOOP ( 'NONE', ( #1413, #8696, #2340, #12588 ) ) ;
#20882 = AXIS2_PLACEMENT_3D ( 'NONE', #12970, #19943, #19819 ) ;
#20883 = CARTESIAN_POINT ( 'NONE',  ( 30.49999999999999645, -84.70000000000001705, 0.3000000000000033751 ) ) ;
#20884 = CIRCLE ( 'NONE', #11938, 0.04999999999999991257 ) ;
#20885 = EDGE_CURVE ( 'NONE', #22148, #9132, #2, .T. ) ;
#20886 = EDGE_LOOP ( 'NONE', ( #14834, #12915, #5882, #13380 ) ) ;
#20887 = DIRECTION ( 'NONE',  ( 1.000000000000000000, 0.000000000000000000, 0.000000000000000000 ) ) ;
#20888 = EDGE_CURVE ( 'NONE', #21066, #9400, #8191, .T. ) ;
#20889 = ORIENTED_EDGE ( 'NONE', *, *, #4591, .T. ) ;
#20890 = DIRECTION ( 'NONE',  ( 0.000000000000000000, -1.000000000000000000, 0.000000000000000000 ) ) ;
#20891 = DIRECTION ( 'NONE',  ( 1.000000000000000000, 0.000000000000000000, 0.000000000000000000 ) ) ;
#20892 = FACE_OUTER_BOUND ( 'NONE', #9370, .T. ) ;
#20893 = LINE ( 'NONE', #17847, #18060 ) ;
#20894 = VERTEX_POINT ( 'NONE', #21841 ) ;
#20895 = DIRECTION ( 'NONE',  ( -2.832483164223434527E-16, -1.000000000000000000, 0.000000000000000000 ) ) ;
#20896 = PLANE ( 'NONE',  #7825 ) ;
#20897 = CARTESIAN_POINT ( 'NONE',  ( 32.20000000000001705, -71.00000000000001421, 3.500000000000000000 ) ) ;
#20898 = DIRECTION ( 'NONE',  ( 0.000000000000000000, -0.000000000000000000, 1.000000000000000000 ) ) ;
#20899 = ORIENTED_EDGE ( 'NONE', *, *, #13247, .F. ) ;
#20900 = CARTESIAN_POINT ( 'NONE',  ( 1.774728116533973665, 42.31054587065082728, 12.00000000000000000 ) ) ;
#20901 = ORIENTED_EDGE ( 'NONE', *, *, #11822, .F. ) ;
#20902 = DIRECTION ( 'NONE',  ( 1.000000000000000000, 0.000000000000000000, 0.000000000000000000 ) ) ;
#20903 = CARTESIAN_POINT ( 'NONE',  ( -1.824728116533986810, 43.31054587065082728, 51.70876104995653577 ) ) ;
#20904 = ORIENTED_EDGE ( 'NONE', *, *, #13436, .T. ) ;
#20905 = ORIENTED_EDGE ( 'NONE', *, *, #3727, .T. ) ;
#20906 = DIRECTION ( 'NONE',  ( 0.000000000000000000, 0.000000000000000000, 1.000000000000000000 ) ) ;
#20907 = EDGE_CURVE ( 'NONE', #19066, #12981, #9331, .T. ) ;
#20908 = CARTESIAN_POINT ( 'NONE',  ( 0.000000000000000000, 42.31054587065082728, 33.71679706732589921 ) ) ;
#20909 = ORIENTED_EDGE ( 'NONE', *, *, #10719, .T. ) ;
#20910 = ORIENTED_EDGE ( 'NONE', *, *, #21199, .F. ) ;
#20911 = AXIS2_PLACEMENT_3D ( 'NONE', #12592, #18690, #10926 ) ;
#20912 = VECTOR ( 'NONE', #16004, 1000.000000000000000 ) ;
#20913 = ADVANCED_FACE ( 'NONE', ( #18457 ), #10085, .T. ) ;
#20914 = ORIENTED_EDGE ( 'NONE', *, *, #14069, .F. ) ;
#20915 = DIRECTION ( 'NONE',  ( 0.4461977533474359436, 1.454668808886071847E-15, -0.8949343913984424415 ) ) ;
#20916 = DIRECTION ( 'NONE',  ( -0.000000000000000000, 0.000000000000000000, 1.000000000000000000 ) ) ;
#20917 = CARTESIAN_POINT ( 'NONE',  ( -27.67540678000427690, 10.94079601157914539, 13.79999999999999893 ) ) ;
#20918 = VERTEX_POINT ( 'NONE', #13647 ) ;
#20919 = CARTESIAN_POINT ( 'NONE',  ( 14.75227361591076836, 52.14371094704549847, 13.50000000000000000 ) ) ;
#20920 = DIRECTION ( 'NONE',  ( -1.000000000000000000, 0.000000000000000000, 0.000000000000000000 ) ) ;
#20921 = CARTESIAN_POINT ( 'NONE',  ( -3.127054932750481964, -32.11873716947361856, 109.6002446535588319 ) ) ;
#20922 = AXIS2_PLACEMENT_3D ( 'NONE', #3542, #20546, #10369 ) ;
#20923 = AXIS2_PLACEMENT_3D ( 'NONE', #5476, #14055, #18194 ) ;
#20924 = ORIENTED_EDGE ( 'NONE', *, *, #4174, .T. ) ;
#20925 = EDGE_CURVE ( 'NONE', #1152, #21509, #8516, .T. ) ;
#20926 = CARTESIAN_POINT ( 'NONE',  ( -1.824728116533986810, 42.36054587065083155, 39.75876104995654003 ) ) ;
#20927 = ORIENTED_EDGE ( 'NONE', *, *, #9038, .T. ) ;
#20928 = EDGE_CURVE ( 'NONE', #5745, #18705, #6128, .T. ) ;
#20929 = ORIENTED_EDGE ( 'NONE', *, *, #4515, .T. ) ;
#20930 = EDGE_LOOP ( 'NONE', ( #14060, #11043, #12789, #20242 ) ) ;
#20931 = LINE ( 'NONE', #12517, #3893 ) ;
#20932 = CONTEXT_DEPENDENT_SHAPE_REPRESENTATION ( #11437, #12153 ) ;
#20933 = VERTEX_POINT ( 'NONE', #15206 ) ;
#20934 = ORIENTED_EDGE ( 'NONE', *, *, #14305, .T. ) ;
#20935 = CIRCLE ( 'NONE', #17685, 0.04999999999999991257 ) ;
#20936 = CARTESIAN_POINT ( 'NONE',  ( 23.02398829872513986, -2.624711895713193410, 13.63074282194498821 ) ) ;
#20937 = ORIENTED_EDGE ( 'NONE', *, *, #11946, .T. ) ;
#20938 = AXIS2_PLACEMENT_3D ( 'NONE', #21394, #1214, #11184 ) ;
#20939 = AXIS2_PLACEMENT_3D ( 'NONE', #9804, #10248, #2977 ) ;
#20940 = AXIS2_PLACEMENT_3D ( 'NONE', #11356, #1164, #8009 ) ;
#20941 = VERTEX_POINT ( 'NONE', #15330 ) ;
#20942 = DIRECTION ( 'NONE',  ( 0.000000000000000000, -1.000000000000000000, 0.000000000000000000 ) ) ;
#20943 = FACE_OUTER_BOUND ( 'NONE', #9542, .T. ) ;
#20944 = CARTESIAN_POINT ( 'NONE',  ( -17.95292532278785913, 34.11873716947361856, 68.00000000000000000 ) ) ;
#20945 = EDGE_CURVE ( 'NONE', #18066, #8501, #3255, .T. ) ;
#20946 = DIRECTION ( 'NONE',  ( -1.000000000000000000, 3.009265538104883829E-28, -4.336808689941893885E-15 ) ) ;
#20947 = CARTESIAN_POINT ( 'NONE',  ( 28.57540678000427548, 6.776800961815481195, 13.50000000000000000 ) ) ;
#20948 = DIRECTION ( 'NONE',  ( -0.000000000000000000, 0.000000000000000000, 1.000000000000000000 ) ) ;
#20949 = DIRECTION ( 'NONE',  ( -1.224646799147353207E-16, -0.000000000000000000, -1.000000000000000000 ) ) ;
#20950 = VECTOR ( 'NONE', #17736, 1000.000000000000000 ) ;
#20951 = AXIS2_PLACEMENT_3D ( 'NONE', #20752, #21086, #19065 ) ;
#20952 = VECTOR ( 'NONE', #19865, 1000.000000000000000 ) ;
#20953 = EDGE_CURVE ( 'NONE', #11867, #8198, #11852, .T. ) ;
#20954 = CARTESIAN_POINT ( 'NONE',  ( -15.13056916446893396, -52.10286008774955491, 13.87500000000000178 ) ) ;
#20955 = VERTEX_POINT ( 'NONE', #1086 ) ;
#20956 = AXIS2_PLACEMENT_3D ( 'NONE', #3527, #10358, #17166 ) ;
#20957 = CARTESIAN_POINT ( 'NONE',  ( 9.141460742840918030, 33.43424481021354921, 68.00000000000000000 ) ) ;
#20958 =( NAMED_UNIT ( * ) PLANE_ANGLE_UNIT ( ) SI_UNIT ( $, .RADIAN. ) );
#20959 = CARTESIAN_POINT ( 'NONE',  ( 29.50000000000002132, 0.000000000000000000, 1.500000000000000000 ) ) ;
#20960 = ORIENTED_EDGE ( 'NONE', *, *, #3916, .F. ) ;
#20961 = ORIENTED_EDGE ( 'NONE', *, *, #5844, .T. ) ;
#20962 = AXIS2_PLACEMENT_3D ( 'NONE', #14468, #7347, #722 ) ;
#20963 = AXIS2_PLACEMENT_3D ( 'NONE', #9457, #7800, #9908 ) ;
#20964 = AXIS2_PLACEMENT_3D ( 'NONE', #4551, #9467, #7923 ) ;
#20965 = TOROIDAL_SURFACE ( 'NONE', #17725, 0.5999999999999999778, 0.2999999999999999889 ) ;
#20966 = EDGE_CURVE ( 'NONE', #8457, #14272, #2652, .T. ) ;
#20967 = CARTESIAN_POINT ( 'NONE',  ( -29.13662752439705272, 0.000000000000000000, 7.500000000000000000 ) ) ;
#20968 = CARTESIAN_POINT ( 'NONE',  ( 29.50000000000002132, -69.00000000000000000, -150.0833101980363722 ) ) ;
#20969 = CIRCLE ( 'NONE', #5255, 6.800000000000000711 ) ;
#20970 = ORIENTED_EDGE ( 'NONE', *, *, #17595, .F. ) ;
#20971 = CYLINDRICAL_SURFACE ( 'NONE', #16060, 2.000000000000000000 ) ;
#20972 = LINE ( 'NONE', #3859, #3179 ) ;
#20973 = DIRECTION ( 'NONE',  ( -1.000000000000000000, 0.000000000000000000, 0.000000000000000000 ) ) ;
#20974 = LINE ( 'NONE', #10562, #2123 ) ;
#20975 = CARTESIAN_POINT ( 'NONE',  ( 1.724728116533979616, 43.31054587065082728, 43.80876104995653719 ) ) ;
#20976 = CARTESIAN_POINT ( 'NONE',  ( -27.37540678000427619, 5.683640910026986681, 13.50000000000000000 ) ) ;
#20977 = EDGE_CURVE ( 'NONE', #19696, #9561, #2993, .T. ) ;
#20978 = ADVANCED_FACE ( 'NONE', ( #9820 ), #15746, .T. ) ;
#20979 = DIRECTION ( 'NONE',  ( 0.000000000000000000, 0.000000000000000000, 1.000000000000000000 ) ) ;
#20980 = CARTESIAN_POINT ( 'NONE',  ( -14.66174975910705136, 42.11054587065083155, 13.50000000000000000 ) ) ;
#20981 = AXIS2_PLACEMENT_3D ( 'NONE', #8337, #16936, #13788 ) ;
#20982 = ADVANCED_FACE ( 'NONE', ( #21479 ), #13277, .T. ) ;
#20983 = FACE_OUTER_BOUND ( 'NONE', #664, .T. ) ;
#20984 = ORIENTED_EDGE ( 'NONE', *, *, #11674, .F. ) ;
#20985 = AXIS2_PLACEMENT_3D ( 'NONE', #21717, #1544, #13408 ) ;
#20986 = CIRCLE ( 'NONE', #11317, 0.5000000000000004441 ) ;
#20987 = EDGE_LOOP ( 'NONE', ( #6327, #3075, #12336, #20960 ) ) ;
#20988 = ORIENTED_EDGE ( 'NONE', *, *, #12169, .F. ) ;
#20989 = PLANE ( 'NONE',  #11696 ) ;
#20990 = DIRECTION ( 'NONE',  ( 0.000000000000000000, -1.000000000000000000, 0.000000000000000000 ) ) ;
#20991 = AXIS2_PLACEMENT_3D ( 'NONE', #20917, #9730, #14509 ) ;
#20992 = EDGE_LOOP ( 'NONE', ( #5739, #9439 ) ) ;
#20993 = TOROIDAL_SURFACE ( 'NONE', #19976, 2.800000000000002043, 0.2999999999999999889 ) ;
#20994 = AXIS2_PLACEMENT_3D ( 'NONE', #17864, #19135, #2542 ) ;
#20995 = ORIENTED_EDGE ( 'NONE', *, *, #8049, .F. ) ;
#20996 = FACE_OUTER_BOUND ( 'NONE', #10780, .T. ) ;
#20997 = LINE ( 'NONE', #14266, #15231 ) ;
#20998 = EDGE_CURVE ( 'NONE', #9803, #620, #18614, .T. ) ;
#20999 = ORIENTED_EDGE ( 'NONE', *, *, #1580, .T. ) ;
#21000 = CYLINDRICAL_SURFACE ( 'NONE', #8169, 0.2500000000000001665 ) ;
#21001 = FACE_OUTER_BOUND ( 'NONE', #5861, .T. ) ;
#21002 = CIRCLE ( 'NONE', #14558, 0.5000000000000004441 ) ;
#21003 = AXIS2_PLACEMENT_3D ( 'NONE', #15073, #21917, #16749 ) ;
#21004 = AXIS2_PLACEMENT_3D ( 'NONE', #17128, #16900, #1564 ) ;
#21005 = DIRECTION ( 'NONE',  ( -0.000000000000000000, 1.000000000000000000, -0.000000000000000000 ) ) ;
#21006 = FACE_OUTER_BOUND ( 'NONE', #8436, .T. ) ;
#21007 = EDGE_LOOP ( 'NONE', ( #9819, #8623, #7976, #8995 ) ) ;
#21008 = DIRECTION ( 'NONE',  ( 2.107255972849994642E-16, -0.000000000000000000, 1.000000000000000000 ) ) ;
#21009 = DIRECTION ( 'NONE',  ( 1.000000000000000000, 0.000000000000000000, 0.000000000000000000 ) ) ;
#21010 = CIRCLE ( 'NONE', #19217, 0.2500000000000002220 ) ;
#21011 = DIRECTION ( 'NONE',  ( 1.000000000000000000, 0.000000000000000000, 0.000000000000000000 ) ) ;
#21012 = CARTESIAN_POINT ( 'NONE',  ( 25.37540678000429040, -36.74634676501047181, 42.50000000000000000 ) ) ;
#21013 = VERTEX_POINT ( 'NONE', #12825 ) ;
#21014 = CARTESIAN_POINT ( 'NONE',  ( 1.824728116533979261, 43.26054587065083012, 27.80876104995653719 ) ) ;
#21015 = CIRCLE ( 'NONE', #11346, 0.1000000000000028644 ) ;
#21016 = VECTOR ( 'NONE', #11197, 1000.000000000000000 ) ;
#21017 = EDGE_CURVE ( 'NONE', #16490, #9069, #4709, .T. ) ;
#21018 = ORIENTED_EDGE ( 'NONE', *, *, #654, .F. ) ;
#21019 = CARTESIAN_POINT ( 'NONE',  ( -14.71174975910705029, 52.11873716947361856, 109.6002446535588319 ) ) ;
#21020 = EDGE_CURVE ( 'NONE', #2890, #11049, #16417, .T. ) ;
#21021 = CARTESIAN_POINT ( 'NONE',  ( 0.000000000000000000, -39.04634676501046187, 13.79999999999999893 ) ) ;
#21022 = EDGE_LOOP ( 'NONE', ( #14783, #9206, #21533, #18024 ) ) ;
#21023 = ORIENTED_EDGE ( 'NONE', *, *, #15603, .F. ) ;
#21024 = EDGE_CURVE ( 'NONE', #5793, #16645, #12529, .T. ) ;
#21025 = CARTESIAN_POINT ( 'NONE',  ( -8.134906293162361024, 41.92645089659918511, 68.06527860057354928 ) ) ;
#21026 = VECTOR ( 'NONE', #15324, 1000.000000000000000 ) ;
#21027 = VECTOR ( 'NONE', #12674, 1000.000000000000000 ) ;
#21028 = VECTOR ( 'NONE', #15188, 1000.000000000000000 ) ;
#21029 = EDGE_LOOP ( 'NONE', ( #19484, #15115, #5114, #4403 ) ) ;
#21030 = AXIS2_PLACEMENT_3D ( 'NONE', #15967, #14400, #7609 ) ;
#21031 = VERTEX_POINT ( 'NONE', #13169 ) ;
#21032 = AXIS2_PLACEMENT_3D ( 'NONE', #18813, #8406, #13659 ) ;
#21033 = AXIS2_PLACEMENT_3D ( 'NONE', #2412, #830, #17845 ) ;
#21034 =( REPRESENTATION_RELATIONSHIP ('NONE','NONE', #561, #9142 ) REPRESENTATION_RELATIONSHIP_WITH_TRANSFORMATION ( #12518 )SHAPE_REPRESENTATION_RELATIONSHIP( ) );
#21035 = ADVANCED_FACE ( 'NONE', ( #21588 ), #3628, .T. ) ;
#21036 = DIRECTION ( 'NONE',  ( -0.000000000000000000, 1.000000000000000000, -0.000000000000000000 ) ) ;
#21037 = CARTESIAN_POINT ( 'NONE',  ( -15.21174975910705207, -32.10873716947361345, 68.25000000000000000 ) ) ;
#21038 = CYLINDRICAL_SURFACE ( 'NONE', #11862, 0.2500000000000002220 ) ;
#21039 = DIRECTION ( 'NONE',  ( 1.000000000000000000, 0.000000000000000000, 0.000000000000000000 ) ) ;
#21040 = EDGE_CURVE ( 'NONE', #706, #8846, #6503, .T. ) ;
#21041 = DIRECTION ( 'NONE',  ( -1.000000000000000000, 0.000000000000000000, 0.000000000000000000 ) ) ;
#21042 = ORIENTED_EDGE ( 'NONE', *, *, #15370, .T. ) ;
#21043 = AXIS2_PLACEMENT_3D ( 'NONE', #20967, #2046, #5766 ) ;
#21044 = CIRCLE ( 'NONE', #5328, 1.000000000000000888 ) ;
#21045 = CARTESIAN_POINT ( 'NONE',  ( -1.824728116533986810, 42.36054587065083155, 39.70876104995653577 ) ) ;
#21046 = FACE_BOUND ( 'NONE', #2342, .T. ) ;
#21047 = CIRCLE ( 'NONE', #9604, 1.000000000000000000 ) ;
#21048 = CARTESIAN_POINT ( 'NONE',  ( -21.92816239687475743, 42.46645089659918426, 13.74999999999999822 ) ) ;
#21049 = AXIS2_PLACEMENT_3D ( 'NONE', #6218, #4410, #2400 ) ;
#21050 = AXIS2_PLACEMENT_3D ( 'NONE', #7956, #11282, #4588 ) ;
#21051 = CIRCLE ( 'NONE', #16747, 0.2999999999999999889 ) ;
#21052 = ADVANCED_FACE ( 'NONE', ( #18085 ), #7827, .T. ) ;
#21053 = ORIENTED_EDGE ( 'NONE', *, *, #18237, .F. ) ;
#21054 = DIRECTION ( 'NONE',  ( -0.000000000000000000, -0.000000000000000000, -1.000000000000000000 ) ) ;
#21055 = VERTEX_POINT ( 'NONE', #16522 ) ;
#21056 = EDGE_LOOP ( 'NONE', ( #17242, #5941, #20851, #14695 ) ) ;
#21057 = ORIENTED_EDGE ( 'NONE', *, *, #13941, .F. ) ;
#21058 = DIRECTION ( 'NONE',  ( -1.000000000000000000, 0.000000000000000000, -0.000000000000000000 ) ) ;
#21059 = ORIENTED_EDGE ( 'NONE', *, *, #11970, .T. ) ;
#21060 = ORIENTED_EDGE ( 'NONE', *, *, #4283, .F. ) ;
#21061 = AXIS2_PLACEMENT_3D ( 'NONE', #6265, #8046, #13052 ) ;
#21062 = CARTESIAN_POINT ( 'NONE',  ( 23.02398829872513986, -3.528912754968634768, 13.50000000000000000 ) ) ;
#21063 = VERTEX_POINT ( 'NONE', #4346 ) ;
#21064 = LINE ( 'NONE', #17791, #6470 ) ;
#21065 = AXIS2_PLACEMENT_3D ( 'NONE', #19532, #4214, #11034 ) ;
#21066 = VERTEX_POINT ( 'NONE', #1186 ) ;
#21067 = AXIS2_PLACEMENT_3D ( 'NONE', #19249, #10519, #8842 ) ;
#21068 = CARTESIAN_POINT ( 'NONE',  ( 1.724728116533979616, 42.36054587065083155, 35.70876104995653577 ) ) ;
#21069 = EDGE_CURVE ( 'NONE', #17577, #19547, #14835, .T. ) ;
#21070 = DIRECTION ( 'NONE',  ( 1.000000000000000000, 0.000000000000000000, 0.000000000000000000 ) ) ;
#21071 = DIRECTION ( 'NONE',  ( 0.000000000000000000, 0.000000000000000000, -1.000000000000000000 ) ) ;
#21072 = ADVANCED_FACE ( 'NONE', ( #20016 ), #15408, .T. ) ;
#21073 = EDGE_CURVE ( 'NONE', #21768, #14801, #2172, .T. ) ;
#21074 = DIRECTION ( 'NONE',  ( -0.000000000000000000, -1.000000000000000000, -0.000000000000000000 ) ) ;
#21075 = CARTESIAN_POINT ( 'NONE',  ( 28.86382559268571057, 6.505889654322387194, 13.29319881794719294 ) ) ;
#21076 = CARTESIAN_POINT ( 'NONE',  ( 0.000000000000000000, 69.00000000000000000, 0.2999999999999947153 ) ) ;
#21077 = CARTESIAN_POINT ( 'NONE',  ( -27.37540678000427619, 10.94079601157914539, 13.79999999999999893 ) ) ;
#21078 = PLANE ( 'NONE',  #17173 ) ;
#21079 = CIRCLE ( 'NONE', #7156, 3.800000000000004707 ) ;
#21080 = EDGE_LOOP ( 'NONE', ( #5834, #12307, #6112, #3958 ) ) ;
#21081 = ORIENTED_EDGE ( 'NONE', *, *, #19015, .F. ) ;
#21082 = DIRECTION ( 'NONE',  ( -1.224646799147353207E-16, -1.000000000000000000, 1.499759782661857608E-32 ) ) ;
#21083 = SHAPE_REPRESENTATION_RELATIONSHIP ( 'NONE' , 'NONE' ,  #6277, #16315 ) ;
#21084 = ORIENTED_EDGE ( 'NONE', *, *, #12589, .T. ) ;
#21085 = ORIENTED_EDGE ( 'NONE', *, *, #9863, .F. ) ;
#21086 = DIRECTION ( 'NONE',  ( -1.000000000000000000, 0.000000000000000000, 0.000000000000000000 ) ) ;
#21087 = VERTEX_POINT ( 'NONE', #856 ) ;
#21088 = EDGE_CURVE ( 'NONE', #7987, #8010, #6038, .T. ) ;
#21089 = CIRCLE ( 'NONE', #1786, 0.5000000000000004441 ) ;
#21090 = PLANE ( 'NONE',  #6700 ) ;
#21091 = AXIS2_PLACEMENT_3D ( 'NONE', #5186, #13769, #20742 ) ;
#21092 = AXIS2_PLACEMENT_3D ( 'NONE', #22140, #4888, #6690 ) ;
#21093 = EDGE_CURVE ( 'NONE', #20918, #1592, #7195, .T. ) ;
#21094 = CARTESIAN_POINT ( 'NONE',  ( -1.774728116533986766, 43.26054587065083012, 4.000000000000000000 ) ) ;
#21095 = ORIENTED_EDGE ( 'NONE', *, *, #8296, .T. ) ;
#21096 = DIRECTION ( 'NONE',  ( -0.000000000000000000, -0.000000000000000000, 1.000000000000000000 ) ) ;
#21097 = CARTESIAN_POINT ( 'NONE',  ( 23.04692967985606700, 2.284552260428339032, 13.25236378595242392 ) ) ;
#21098 = FACE_OUTER_BOUND ( 'NONE', #19511, .T. ) ;
#21099 = DIRECTION ( 'NONE',  ( -0.000000000000000000, -1.000000000000000000, -0.000000000000000000 ) ) ;
#21100 = LINE ( 'NONE', #18037, #11992 ) ;
#21101 = ORIENTED_EDGE ( 'NONE', *, *, #7693, .T. ) ;
#21102 = DIRECTION ( 'NONE',  ( 0.000000000000000000, 0.000000000000000000, 1.000000000000000000 ) ) ;
#21103 = DIRECTION ( 'NONE',  ( 0.000000000000000000, 0.000000000000000000, 1.000000000000000000 ) ) ;
#21104 = FACE_OUTER_BOUND ( 'NONE', #2091, .T. ) ;
#21105 = EDGE_LOOP ( 'NONE', ( #2611, #18933, #4850, #327 ) ) ;
#21106 = ORIENTED_EDGE ( 'NONE', *, *, #17161, .F. ) ;
#21107 = ORIENTED_EDGE ( 'NONE', *, *, #10827, .T. ) ;
#21108 = DIRECTION ( 'NONE',  ( 1.000000000000000000, 0.000000000000000000, -0.000000000000000000 ) ) ;
#21109 = AXIS2_PLACEMENT_3D ( 'NONE', #18506, #21989, #3404 ) ;
#21110 = CARTESIAN_POINT ( 'NONE',  ( 9.641460742840918030, 32.61873716947361856, 68.00000000000000000 ) ) ;
#21111 = ORIENTED_EDGE ( 'NONE', *, *, #4398, .F. ) ;
#21112 = AXIS2_PLACEMENT_3D ( 'NONE', #21995, #1842, #17056 ) ;
#21113 = EDGE_CURVE ( 'NONE', #6391, #9883, #13613, .T. ) ;
#21114 = CARTESIAN_POINT ( 'NONE',  ( 1.774728116533973665, 43.26054587065083012, 20.00000000000000000 ) ) ;
#21115 = ORIENTED_EDGE ( 'NONE', *, *, #11066, .T. ) ;
#21116 = DIRECTION ( 'NONE',  ( 0.000000000000000000, 0.000000000000000000, 1.000000000000000000 ) ) ;
#21117 = FACE_OUTER_BOUND ( 'NONE', #15689, .T. ) ;
#21118 = ADVANCED_FACE ( 'NONE', ( #8704 ), #12140, .T. ) ;
#21119 = ORIENTED_EDGE ( 'NONE', *, *, #20754, .T. ) ;
#21120 = CARTESIAN_POINT ( 'NONE',  ( -28.64417692495746692, -6.713479613976641502, 13.50000000000000000 ) ) ;
#21121 = DIRECTION ( 'NONE',  ( 0.000000000000000000, 1.000000000000000000, 0.000000000000000000 ) ) ;
#21122 = CYLINDRICAL_SURFACE ( 'NONE', #20090, 4.351418481279137218 ) ;
#21123 = DIRECTION ( 'NONE',  ( 0.000000000000000000, 0.000000000000000000, 1.000000000000000000 ) ) ;
#21124 = ORIENTED_EDGE ( 'NONE', *, *, #5123, .F. ) ;
#21125 = CARTESIAN_POINT ( 'NONE',  ( -21.67365502786443088, 45.72430987248279166, 13.74999999999999822 ) ) ;
#21126 = DIRECTION ( 'NONE',  ( -1.000000000000000000, 0.000000000000000000, 0.000000000000000000 ) ) ;
#21127 = AXIS2_PLACEMENT_3D ( 'NONE', #4546, #18302, #8019 ) ;
#21128 = CIRCLE ( 'NONE', #16805, 1.000000000000000888 ) ;
#21129 = LINE ( 'NONE', #15834, #10861 ) ;
#21130 = DIRECTION ( 'NONE',  ( -0.000000000000000000, -0.000000000000000000, -1.000000000000000000 ) ) ;
#21131 = ORIENTED_EDGE ( 'NONE', *, *, #9815, .T. ) ;
#21132 = SURFACE_STYLE_USAGE ( .BOTH. , #5579 ) ;
#21133 = ORIENTED_EDGE ( 'NONE', *, *, #14958, .F. ) ;
#21134 = LINE ( 'NONE', #12689, #15534 ) ;
#21135 = DIRECTION ( 'NONE',  ( 0.000000000000000000, -0.000000000000000000, 1.000000000000000000 ) ) ;
#21136 = ORIENTED_EDGE ( 'NONE', *, *, #5256, .F. ) ;
#21137 = EDGE_LOOP ( 'NONE', ( #14102, #7904, #13709, #1685 ) ) ;
#21138 = CARTESIAN_POINT ( 'NONE',  ( -9.178906393579158163, 42.46645089659918426, 70.88527860057354246 ) ) ;
#21139 = EDGE_CURVE ( 'NONE', #8815, #6391, #5050, .T. ) ;
#21140 = CARTESIAN_POINT ( 'NONE',  ( -15.21174975910705207, 41.81054587065082728, 68.50000000000000000 ) ) ;
#21141 = ORIENTED_EDGE ( 'NONE', *, *, #16280, .T. ) ;
#21142 = AXIS2_PLACEMENT_3D ( 'NONE', #13817, #18647, #1630 ) ;
#21143 = VERTEX_POINT ( 'NONE', #20558 ) ;
#21144 = EDGE_CURVE ( 'NONE', #21013, #10999, #6697, .T. ) ;
#21145 = EDGE_CURVE ( 'NONE', #7850, #7284, #6926, .T. ) ;
#21146 = CARTESIAN_POINT ( 'NONE',  ( -29.69597781366221412, 27.99124249474150972, 68.75000000000000000 ) ) ;
#21147 = DIRECTION ( 'NONE',  ( 0.000000000000000000, 0.000000000000000000, 1.000000000000000000 ) ) ;
#21148 = CIRCLE ( 'NONE', #8283, 0.5000000000000004441 ) ;
#21149 = EDGE_CURVE ( 'NONE', #1748, #2230, #17192, .T. ) ;
#21150 = DIRECTION ( 'NONE',  ( -1.000000000000000000, 0.000000000000000000, -0.000000000000000000 ) ) ;
#21151 = EDGE_CURVE ( 'NONE', #13818, #18447, #3554, .T. ) ;
#21152 = CARTESIAN_POINT ( 'NONE',  ( 25.37540678000427263, 63.74634676501045050, 7.500000000000000000 ) ) ;
#21153 = AXIS2_PLACEMENT_3D ( 'NONE', #19183, #11003, #2275 ) ;
#21154 = DIRECTION ( 'NONE',  ( 0.000000000000000000, -0.000000000000000000, -1.000000000000000000 ) ) ;
#21155 = DIRECTION ( 'NONE',  ( 1.000000000000000000, 0.000000000000000000, 0.000000000000000000 ) ) ;
#21156 = ORIENTED_EDGE ( 'NONE', *, *, #16663, .T. ) ;
#21157 = CARTESIAN_POINT ( 'NONE',  ( 14.66174975910705847, 51.84675762924570108, 13.50000000000000355 ) ) ;
#21158 = CARTESIAN_POINT ( 'NONE',  ( -30.79999999999999361, -84.70000000000001705, 0.3000000000000002665 ) ) ;
#21159 = DIRECTION ( 'NONE',  ( 0.000000000000000000, 0.000000000000000000, 1.000000000000000000 ) ) ;
#21160 = VERTEX_POINT ( 'NONE', #1526 ) ;
#21161 = ADVANCED_FACE ( 'NONE', ( #22145 ), #14644, .T. ) ;
#21162 = CARTESIAN_POINT ( 'NONE',  ( -31.69597781366221412, 27.99124249474150972, 70.25000000000000000 ) ) ;
#21163 = VERTEX_POINT ( 'NONE', #5122 ) ;
#21164 = CIRCLE ( 'NONE', #17215, 0.5000000000000004441 ) ;
#21165 = EDGE_LOOP ( 'NONE', ( #20074, #8792, #17640, #15055 ) ) ;
#21166 = EDGE_LOOP ( 'NONE', ( #2850, #16354, #16844, #13039 ) ) ;
#21167 = CARTESIAN_POINT ( 'NONE',  ( -3.127054932750481964, 32.61873716947361856, 109.6002446535588319 ) ) ;
#21168 = ITEM_DEFINED_TRANSFORMATION ( 'NONE', 'NONE', #14403,  #17493 ) ;
#21169 = CIRCLE ( 'NONE', #10805, 0.05000000000000143219 ) ;
#21170 = ORIENTED_EDGE ( 'NONE', *, *, #1073, .T. ) ;
#21171 = AXIS2_PLACEMENT_3D ( 'NONE', #20317, #1609, #1506 ) ;
#21172 = VERTEX_POINT ( 'NONE', #13707 ) ;
#21173 = AXIS2_PLACEMENT_3D ( 'NONE', #19587, #17789, #2676 ) ;
#21174 = DIRECTION ( 'NONE',  ( -0.000000000000000000, -0.000000000000000000, -1.000000000000000000 ) ) ;
#21175 = EDGE_LOOP ( 'NONE', ( #16175, #10847, #4396, #18371 ) ) ;
#21176 = LINE ( 'NONE', #10458, #3594 ) ;
#21177 = EDGE_CURVE ( 'NONE', #18812, #2320, #394, .T. ) ;
#21178 = EDGE_LOOP ( 'NONE', ( #1758, #1376, #11922, #8964 ) ) ;
#21179 = EDGE_CURVE ( 'NONE', #15951, #17181, #4344, .T. ) ;
#21180 = DIRECTION ( 'NONE',  ( 0.000000000000000000, 0.000000000000000000, -1.000000000000000000 ) ) ;
#21181 = DIRECTION ( 'NONE',  ( -0.000000000000000000, 0.000000000000000000, 1.000000000000000000 ) ) ;
#21182 = DIRECTION ( 'NONE',  ( 0.000000000000000000, 0.000000000000000000, 1.000000000000000000 ) ) ;
#21183 = DIRECTION ( 'NONE',  ( 1.000000000000000000, 0.000000000000000000, -0.000000000000000000 ) ) ;
#21184 = TOROIDAL_SURFACE ( 'NONE', #11513, 1.000000000000000000, 0.5000000000000000000 ) ;
#21185 = PLANE ( 'NONE',  #442 ) ;
#21186 = VECTOR ( 'NONE', #11264, 1000.000000000000000 ) ;
#21187 = PLANE ( 'NONE',  #9363 ) ;
#21188 = CARTESIAN_POINT ( 'NONE',  ( -1.836970198721029934E-16, 72.00000000000001421, 3.500000000000000000 ) ) ;
#21189 = DIRECTION ( 'NONE',  ( -0.2309407893632117181, 0.9729678061520313781, 0.000000000000000000 ) ) ;
#21190 = PLANE ( 'NONE',  #16655 ) ;
#21191 = VERTEX_POINT ( 'NONE', #8258 ) ;
#21192 = EDGE_LOOP ( 'NONE', ( #4514, #11221, #8768, #20526 ) ) ;
#21193 = CARTESIAN_POINT ( 'NONE',  ( 29.17540678000427690, 0.000000000000000000, 7.500000000000000000 ) ) ;
#21194 = VECTOR ( 'NONE', #3385, 1000.000000000000000 ) ;
#21195 = EDGE_CURVE ( 'NONE', #20541, #16405, #1414, .T. ) ;
#21196 = EDGE_CURVE ( 'NONE', #15364, #4630, #18760, .T. ) ;
#21197 = ORIENTED_EDGE ( 'NONE', *, *, #11279, .F. ) ;
#21198 = ORIENTED_EDGE ( 'NONE', *, *, #4055, .F. ) ;
#21199 = EDGE_CURVE ( 'NONE', #421, #8448, #18627, .T. ) ;
#21200 = DIRECTION ( 'NONE',  ( 0.000000000000000000, 1.000000000000000000, 0.000000000000000000 ) ) ;
#21201 = DIRECTION ( 'NONE',  ( -0.000000000000000000, -0.000000000000000000, -1.000000000000000000 ) ) ;
#21202 = ORIENTED_EDGE ( 'NONE', *, *, #66, .F. ) ;
#21203 = FACE_OUTER_BOUND ( 'NONE', #6500, .T. ) ;
#21204 = DIRECTION ( 'NONE',  ( 0.000000000000000000, -1.000000000000000000, -0.000000000000000000 ) ) ;
#21205 = CARTESIAN_POINT ( 'NONE',  ( 28.87540678000427619, 63.74634676501045050, 13.19999999999999929 ) ) ;
#21206 = CARTESIAN_POINT ( 'NONE',  ( -15.21174975910705207, -51.61873716947361856, 68.00000000000000000 ) ) ;
#21207 = FACE_OUTER_BOUND ( 'NONE', #19671, .T. ) ;
#21208 = ORIENTED_EDGE ( 'NONE', *, *, #20228, .T. ) ;
#21209 = LINE ( 'NONE', #9010, #20427 ) ;
#21210 = DIRECTION ( 'NONE',  ( -0.000000000000000000, -0.000000000000000000, -1.000000000000000000 ) ) ;
#21211 = DIRECTION ( 'NONE',  ( 0.000000000000000000, 0.000000000000000000, 1.000000000000000000 ) ) ;
#21212 = EDGE_LOOP ( 'NONE', ( #13931, #613, #3320, #5097 ) ) ;
#21213 = ORIENTED_EDGE ( 'NONE', *, *, #12114, .T. ) ;
#21214 = ORIENTED_EDGE ( 'NONE', *, *, #4685, .F. ) ;
#21215 = LINE ( 'NONE', #8907, #3852 ) ;
#21217 = EDGE_CURVE ( 'NONE', #9468, #12543, #20343, .T. ) ;
#21216 = CARTESIAN_POINT ( 'NONE',  ( 18.05178606074127501, 38.87061083372239523, 13.49999999999999822 ) ) ;
#21218 = EDGE_LOOP ( 'NONE', ( #2912, #15539, #2445, #5211 ) ) ;
#21219 = EDGE_CURVE ( 'NONE', #21351, #16066, #10014, .T. ) ;
#21220 = CARTESIAN_POINT ( 'NONE',  ( 1.824728116533979705, 43.26054587065083012, 45.66679706732590205 ) ) ;
#21221 = ORIENTED_EDGE ( 'NONE', *, *, #1435, .T. ) ;
#21222 = DIRECTION ( 'NONE',  ( 0.000000000000000000, 0.000000000000000000, 1.000000000000000000 ) ) ;
#21223 = CARTESIAN_POINT ( 'NONE',  ( -1.724728116533986721, 42.36054587065083155, 37.76679706732590347 ) ) ;
#21224 = FACE_OUTER_BOUND ( 'NONE', #19137, .T. ) ;
#21225 = LINE ( 'NONE', #9455, #5447 ) ;
#21226 = LINE ( 'NONE', #2084, #13062 ) ;
#21227 = ORIENTED_EDGE ( 'NONE', *, *, #8803, .T. ) ;
#21228 = CARTESIAN_POINT ( 'NONE',  ( 1.774728116533973665, 43.26054587065083012, -3.739806423751037426E-16 ) ) ;
#21229 = CARTESIAN_POINT ( 'NONE',  ( -35.00000000000001421, -84.70000000000001705, 79.39999999999999147 ) ) ;
#21230 = CARTESIAN_POINT ( 'NONE',  ( -14.96244602927845335, 51.84405746083547228, 13.82646097708239274 ) ) ;
#21231 = DIRECTION ( 'NONE',  ( 1.000000000000000000, 0.000000000000000000, 0.000000000000000000 ) ) ;
#21232 = EDGE_LOOP ( 'NONE', ( #2016, #2619, #20701, #5092 ) ) ;
#21233 = ADVANCED_FACE ( 'NONE', ( #17084 ), #1759, .T. ) ;
#21234 = DIRECTION ( 'NONE',  ( 0.000000000000000000, 0.000000000000000000, -1.000000000000000000 ) ) ;
#21235 = VERTEX_POINT ( 'NONE', #17188 ) ;
#21236 = CARTESIAN_POINT ( 'NONE',  ( 1.724728116533979838, 43.31054587065082728, 33.71679706732589921 ) ) ;
#21237 = AXIS2_PLACEMENT_3D ( 'NONE', #3027, #16661, #4814 ) ;
#21238 = CARTESIAN_POINT ( 'NONE',  ( -23.02398829872514341, -2.333099608346434373, 13.47123417368287868 ) ) ;
#21239 = EDGE_CURVE ( 'NONE', #2536, #5528, #18475, .T. ) ;
#21240 = ORIENTED_EDGE ( 'NONE', *, *, #2968, .F. ) ;
#21241 = EDGE_LOOP ( 'NONE', ( #4391, #7345, #18260, #16163 ) ) ;
#21242 = DIRECTION ( 'NONE',  ( 1.000000000000000000, 0.000000000000000000, 0.000000000000000000 ) ) ;
#21243 = DIRECTION ( 'NONE',  ( 0.000000000000000000, -1.000000000000000000, 0.000000000000000000 ) ) ;
#21244 = ADVANCED_FACE ( 'NONE', ( #1864 ), #15722, .T. ) ;
#21245 = DIRECTION ( 'NONE',  ( 0.000000000000000000, 0.000000000000000000, 1.000000000000000000 ) ) ;
#21246 = EDGE_LOOP ( 'NONE', ( #7071, #4729, #17980, #19192 ) ) ;
#21247 = ORIENTED_EDGE ( 'NONE', *, *, #18957, .F. ) ;
#21248 = ORIENTED_EDGE ( 'NONE', *, *, #1563, .T. ) ;
#21249 = FACE_OUTER_BOUND ( 'NONE', #3068, .T. ) ;
#21250 = CARTESIAN_POINT ( 'NONE',  ( 0.000000000000000000, 52.11873716947361856, 109.6002446535588319 ) ) ;
#21251 = CARTESIAN_POINT ( 'NONE',  ( -9.641460742840918030, 33.43424481021354921, 68.50000000000000000 ) ) ;
#21252 = DIRECTION ( 'NONE',  ( -0.000000000000000000, -0.000000000000000000, -1.000000000000000000 ) ) ;
#21253 = EDGE_CURVE ( 'NONE', #20038, #2381, #6146, .T. ) ;
#21254 = DIRECTION ( 'NONE',  ( 0.000000000000000000, 0.000000000000000000, 1.000000000000000000 ) ) ;
#21255 = DIRECTION ( 'NONE',  ( 6.123233995736764803E-17, 0.000000000000000000, -1.000000000000000000 ) ) ;
#21256 = ORIENTED_EDGE ( 'NONE', *, *, #2550, .T. ) ;
#21257 = DIRECTION ( 'NONE',  ( 1.000000000000000000, 0.000000000000000000, -0.000000000000000000 ) ) ;
#21258 = CARTESIAN_POINT ( 'NONE',  ( 1.724728116533979616, 43.26054587065083012, 51.70876104995653577 ) ) ;
#21259 = CARTESIAN_POINT ( 'NONE',  ( 23.32398829872514057, -2.157133568460768647, 7.500000000000000000 ) ) ;
#21260 = EDGE_CURVE ( 'NONE', #1813, #7349, #19706, .T. ) ;
#21261 = ADVANCED_FACE ( 'NONE', ( #19417 ), #391, .T. ) ;
#21262 = LINE ( 'NONE', #5611, #10989 ) ;
#21263 = EDGE_LOOP ( 'NONE', ( #7997, #12820 ) ) ;
#21264 = ADVANCED_FACE ( 'NONE', ( #20996 ), #5890, .T. ) ;
#21265 = AXIS2_PLACEMENT_3D ( 'NONE', #15840, #5581, #14057 ) ;
#21266 = ORIENTED_EDGE ( 'NONE', *, *, #8456, .T. ) ;
#21267 = VECTOR ( 'NONE', #8760, 1000.000000000000000 ) ;
#21268 = DIRECTION ( 'NONE',  ( -1.000000000000000000, 0.000000000000000000, 0.000000000000000000 ) ) ;
#21269 = ORIENTED_EDGE ( 'NONE', *, *, #1147, .T. ) ;
#21270 = EDGE_LOOP ( 'NONE', ( #2098, #6139, #15595, #14752 ) ) ;
#21271 = EDGE_CURVE ( 'NONE', #4394, #11281, #19203, .T. ) ;
#21272 = DIRECTION ( 'NONE',  ( -1.000000000000000000, 0.000000000000000000, 0.000000000000000000 ) ) ;
#21273 = ORIENTED_EDGE ( 'NONE', *, *, #1229, .T. ) ;
#21274 = CARTESIAN_POINT ( 'NONE',  ( -1.824728116533986810, 43.31054587065082728, 45.66679706732590205 ) ) ;
#21275 = CARTESIAN_POINT ( 'NONE',  ( 1.724728116533979616, 43.31054587065082728, 51.80876104995653719 ) ) ;
#21276 = CARTESIAN_POINT ( 'NONE',  ( -1.724728116533986721, 42.36054587065083155, 37.66679706732590915 ) ) ;
#21277 = EDGE_CURVE ( 'NONE', #5989, #18470, #15758, .T. ) ;
#21278 = CARTESIAN_POINT ( 'NONE',  ( -1.724728116533986721, 43.26054587065083012, 53.66679706732590915 ) ) ;
#21279 = AXIS2_PLACEMENT_3D ( 'NONE', #6522, #11299, #20153 ) ;
#21280 = AXIS2_PLACEMENT_3D ( 'NONE', #3677, #10496, #17303 ) ;
#21281 = DIRECTION ( 'NONE',  ( -0.000000000000000000, 1.000000000000000000, 0.000000000000000000 ) ) ;
#21282 = DIRECTION ( 'NONE',  ( 0.000000000000000000, 1.000000000000000000, 0.000000000000000000 ) ) ;
#21283 = DIRECTION ( 'NONE',  ( 0.000000000000000000, 0.000000000000000000, 1.000000000000000000 ) ) ;
#21284 = CARTESIAN_POINT ( 'NONE',  ( -3.627054932750481964, 33.43424481021354921, 7.321391277662001151 ) ) ;
#21285 = EDGE_CURVE ( 'NONE', #19220, #17480, #21465, .T. ) ;
#21286 = CARTESIAN_POINT ( 'NONE',  ( 29.13662752439705272, 0.000000000000000000, 13.50000000000000000 ) ) ;
#21287 = EDGE_CURVE ( 'NONE', #18991, #1460, #7163, .T. ) ;
#21288 = CARTESIAN_POINT ( 'NONE',  ( -25.37540678000427263, 66.94634676501046044, 13.50000000000000000 ) ) ;
#21289 = ORIENTED_EDGE ( 'NONE', *, *, #16207, .T. ) ;
#21290 = VECTOR ( 'NONE', #21388, 999.9999999999998863 ) ;
#21291 = VERTEX_POINT ( 'NONE', #9121 ) ;
#21292 = CARTESIAN_POINT ( 'NONE',  ( 17.45292532278785913, -34.11873716947361856, 68.00000000000000000 ) ) ;
#21293 = ADVANCED_FACE ( 'NONE', ( #13932, #7572 ), #7243, .F. ) ;
#21294 = FILL_AREA_STYLE_COLOUR ( '', #20145 ) ;
#21295 = ORIENTED_EDGE ( 'NONE', *, *, #9926, .T. ) ;
#21296 = EDGE_LOOP ( 'NONE', ( #14257, #18631, #3313, #16924 ) ) ;
#21297 = VECTOR ( 'NONE', #6354, 1000.000000000000000 ) ;
#21298 = AXIS2_PLACEMENT_3D ( 'NONE', #14152, #9130, #21123 ) ;
#21299 = VERTEX_POINT ( 'NONE', #10705 ) ;
#21300 = EDGE_CURVE ( 'NONE', #9043, #488, #17521, .T. ) ;
#21301 = CARTESIAN_POINT ( 'NONE',  ( -14.66174975910704958, -51.84664399969962290, 13.50000000000000178 ) ) ;
#21302 = AXIS2_PLACEMENT_3D ( 'NONE', #7633, #2921, #13079 ) ;
#21303 = CIRCLE ( 'NONE', #11284, 0.1000000000000028644 ) ;
#21304 = DIRECTION ( 'NONE',  ( -1.000000000000000000, 0.000000000000000000, 0.000000000000000000 ) ) ;
#21305 = ORIENTED_EDGE ( 'NONE', *, *, #16107, .F. ) ;
#21306 = FILL_AREA_STYLE ('',( #14682 ) ) ;
#21307 = EDGE_CURVE ( 'NONE', #14817, #9924, #15003, .T. ) ;
#21308 = FACE_OUTER_BOUND ( 'NONE', #13701, .T. ) ;
#21309 = CARTESIAN_POINT ( 'NONE',  ( 15.00289696508457915, 51.98500081155935248, 13.86091301037357226 ) ) ;
#21310 = CARTESIAN_POINT ( 'NONE',  ( 14.66174975910705847, 51.76873716947361714, 13.50000000000000000 ) ) ;
#21311 = LINE ( 'NONE', #4297, #14473 ) ;
#21312 = VECTOR ( 'NONE', #2505, 1000.000000000000000 ) ;
#21313 = CIRCLE ( 'NONE', #14146, 3.200000000000001510 ) ;
#21314 = VERTEX_POINT ( 'NONE', #17290 ) ;
#21315 = CARTESIAN_POINT ( 'NONE',  ( -1.774728116533986766, 42.31054587065082728, 20.00000000000000000 ) ) ;
#21316 = DIRECTION ( 'NONE',  ( 0.000000000000000000, 0.000000000000000000, 1.000000000000000000 ) ) ;
#21317 = ORIENTED_EDGE ( 'NONE', *, *, #1972, .T. ) ;
#21318 = VERTEX_POINT ( 'NONE', #495 ) ;
#21319 = VERTEX_POINT ( 'NONE', #15928 ) ;
#21320 = CARTESIAN_POINT ( 'NONE',  ( 14.98852729675275164, 51.95836184682381287, 13.85634242029625973 ) ) ;
#21321 = EDGE_CURVE ( 'NONE', #8649, #20699, #13581, .T. ) ;
#21322 = CARTESIAN_POINT ( 'NONE',  ( -15.21174975910705207, 42.31054587065082728, 68.50000000000000000 ) ) ;
#21323 = ORIENTED_EDGE ( 'NONE', *, *, #14662, .T. ) ;
#21324 = AXIS2_PLACEMENT_3D ( 'NONE', #12356, #1273, #9581 ) ;
#21325 = AXIS2_PLACEMENT_3D ( 'NONE', #21021, #12049, #5708 ) ;
#21326 = CARTESIAN_POINT ( 'NONE',  ( 15.95292532278785913, 52.39333383871510108, 13.50000000000000000 ) ) ;
#21327 = VECTOR ( 'NONE', #885, 1000.000000000000000 ) ;
#21328 = VERTEX_POINT ( 'NONE', #14265 ) ;
#21329 = DIRECTION ( 'NONE',  ( 1.000000000000000000, 0.000000000000000000, 0.000000000000000000 ) ) ;
#21330 = CIRCLE ( 'NONE', #10264, 0.2500000000000002220 ) ;
#21331 = DIRECTION ( 'NONE',  ( 1.000000000000000000, 0.000000000000000000, 0.000000000000000000 ) ) ;
#21332 = DIRECTION ( 'NONE',  ( 0.000000000000000000, -1.000000000000000000, 0.000000000000000000 ) ) ;
#21333 = CARTESIAN_POINT ( 'NONE',  ( -23.02398829872513986, 7.027230193580998154E-15, 42.50000000000000000 ) ) ;
#21334 = CARTESIAN_POINT ( 'NONE',  ( 23.02398829872513986, -3.528912754968634768, 13.79999999999999893 ) ) ;
#21335 = DIRECTION ( 'NONE',  ( -0.000000000000000000, 1.000000000000000000, 0.000000000000000000 ) ) ;
#21336 = VERTEX_POINT ( 'NONE', #8801 ) ;
#21337 = DIRECTION ( 'NONE',  ( 0.000000000000000000, 0.000000000000000000, 1.000000000000000000 ) ) ;
#21338 = DIRECTION ( 'NONE',  ( 0.000000000000000000, 0.000000000000000000, 1.000000000000000000 ) ) ;
#21339 = ADVANCED_FACE ( 'NONE', ( #17621 ), #12464, .T. ) ;
#21340 = DIRECTION ( 'NONE',  ( 0.000000000000000000, 0.000000000000000000, 1.000000000000000000 ) ) ;
#21341 = CARTESIAN_POINT ( 'NONE',  ( 25.37540678000427263, -68.74634676501045760, 3.799999999999999822 ) ) ;
#21342 = ORIENTED_EDGE ( 'NONE', *, *, #11467, .F. ) ;
#21343 = EDGE_CURVE ( 'NONE', #7284, #1910, #12893, .T. ) ;
#21344 = AXIS2_PLACEMENT_3D ( 'NONE', #11134, #16395, #2744 ) ;
#21345 = AXIS2_PLACEMENT_3D ( 'NONE', #18251, #13211, #14456 ) ;
#21346 = CARTESIAN_POINT ( 'NONE',  ( 1.724728116533979616, 43.31054587065082728, 39.80876104995653719 ) ) ;
#21347 = CARTESIAN_POINT ( 'NONE',  ( 0.000000000000000000, 68.74634676501045760, 7.200000000000000178 ) ) ;
#21348 = VECTOR ( 'NONE', #4354, 1000.000000000000000 ) ;
#21349 = EDGE_LOOP ( 'NONE', ( #7561, #668, #13178, #20165 ) ) ;
#21350 = DIRECTION ( 'NONE',  ( 0.000000000000000000, 0.000000000000000000, 1.000000000000000000 ) ) ;
#21351 = VERTEX_POINT ( 'NONE', #18992 ) ;
#21352 = AXIS2_PLACEMENT_3D ( 'NONE', #10476, #5346, #8354 ) ;
#21353 = VERTEX_POINT ( 'NONE', #1956 ) ;
#21354 = DIRECTION ( 'NONE',  ( -2.107255972849994642E-16, 0.000000000000000000, -1.000000000000000000 ) ) ;
#21355 = DIRECTION ( 'NONE',  ( -0.000000000000000000, 0.000000000000000000, -1.000000000000000000 ) ) ;
#21356 = ORIENTED_EDGE ( 'NONE', *, *, #11674, .T. ) ;
#21357 = AXIS2_PLACEMENT_3D ( 'NONE', #17473, #2356, #21071 ) ;
#21358 = ORIENTED_EDGE ( 'NONE', *, *, #5313, .T. ) ;
#21359 = DIRECTION ( 'NONE',  ( 1.000000000000000000, 0.000000000000000000, 0.000000000000000000 ) ) ;
#21360 = TOROIDAL_SURFACE ( 'NONE', #1322, 6.800000000000001599, 0.2999999999999999889 ) ;
#21361 = AXIS2_PLACEMENT_3D ( 'NONE', #20926, #16091, #20825 ) ;
#21362 = ORIENTED_EDGE ( 'NONE', *, *, #21624, .F. ) ;
#21363 = CARTESIAN_POINT ( 'NONE',  ( 1.774728116533979438, 43.31054587065082728, 27.80876104995653719 ) ) ;
#21364 = CIRCLE ( 'NONE', #17780, 0.2500000000000011657 ) ;
#21365 = CARTESIAN_POINT ( 'NONE',  ( 30.19999999999999574, 69.70000000000000284, 1.200000000000003064 ) ) ;
#21366 = CIRCLE ( 'NONE', #10980, 2.000000000000000000 ) ;
#21367 = DIRECTION ( 'NONE',  ( 0.000000000000000000, -1.000000000000000000, 0.000000000000000000 ) ) ;
#21368 = CIRCLE ( 'NONE', #17078, 1.000000000000000888 ) ;
#21369 = LINE ( 'NONE', #17768, #20303 ) ;
#21370 = EDGE_CURVE ( 'NONE', #4394, #1910, #11110, .T. ) ;
#21371 = LINE ( 'NONE', #17987, #10617 ) ;
#21372 = ORIENTED_EDGE ( 'NONE', *, *, #12018, .F. ) ;
#21373 = DIRECTION ( 'NONE',  ( -1.000000000000000000, -0.000000000000000000, -0.000000000000000000 ) ) ;
#21374 = LINE ( 'NONE', #7615, #18189 ) ;
#21375 = CARTESIAN_POINT ( 'NONE',  ( 25.37540678000426908, 39.04634676501046187, 13.50000000000000000 ) ) ;
#21376 = AXIS2_PLACEMENT_3D ( 'NONE', #14738, #1188, #21589 ) ;
#21377 = CIRCLE ( 'NONE', #9577, 2.274596669241485181 ) ;
#21378 = CARTESIAN_POINT ( 'NONE',  ( 30.07540678000427548, 6.000000000000000000, 7.500000000000000000 ) ) ;
#21379 = ORIENTED_EDGE ( 'NONE', *, *, #21529, .F. ) ;
#21380 = CIRCLE ( 'NONE', #1718, 0.5000000000000000000 ) ;
#21381 = VERTEX_POINT ( 'NONE', #18178 ) ;
#21382 = CIRCLE ( 'NONE', #2797, 1.250000000000000222 ) ;
#21383 = DIRECTION ( 'NONE',  ( 1.000000000000000000, 0.000000000000000000, 0.000000000000000000 ) ) ;
#21384 = CIRCLE ( 'NONE', #6025, 0.2500000000000002220 ) ;
#21385 = ITEM_DEFINED_TRANSFORMATION ( 'NONE', 'NONE', #3003,  #17493 ) ;
#21386 = ORIENTED_EDGE ( 'NONE', *, *, #16988, .F. ) ;
#21387 = ORIENTED_EDGE ( 'NONE', *, *, #20001, .F. ) ;
#21388 = DIRECTION ( 'NONE',  ( 0.2309407893632117181, -0.9729678061520313781, -0.000000000000000000 ) ) ;
#21389 = CARTESIAN_POINT ( 'NONE',  ( -29.13662752439705272, 5.299999999999999822, 7.500000000000000000 ) ) ;
#21390 = VERTEX_POINT ( 'NONE', #21447 ) ;
#21391 = FACE_OUTER_BOUND ( 'NONE', #18259, .T. ) ;
#21392 = VECTOR ( 'NONE', #18370, 1000.000000000000000 ) ;
#21393 = EDGE_CURVE ( 'NONE', #15847, #5647, #21559, .T. ) ;
#21394 = CARTESIAN_POINT ( 'NONE',  ( -25.37540678000427263, -63.74634676501045050, 13.19999999999999929 ) ) ;
#21395 = DIRECTION ( 'NONE',  ( -1.000000000000000000, 0.000000000000000000, -0.000000000000000000 ) ) ;
#21396 = CARTESIAN_POINT ( 'NONE',  ( -9.641460742840918030, -32.93424481021354921, 68.00000000000000000 ) ) ;
#21397 = EDGE_CURVE ( 'NONE', #2663, #5552, #11834, .T. ) ;
#21398 = VECTOR ( 'NONE', #4793, 1000.000000000000000 ) ;
#21399 = VECTOR ( 'NONE', #12727, 1000.000000000000000 ) ;
#21400 = CARTESIAN_POINT ( 'NONE',  ( -15.21174975910705207, 42.31054587065082728, 68.25000000000000000 ) ) ;
#21401 = VECTOR ( 'NONE', #6718, 1000.000000000000000 ) ;
#21402 = CYLINDRICAL_SURFACE ( 'NONE', #21613, 0.2500000000000002220 ) ;
#21403 = CARTESIAN_POINT ( 'NONE',  ( -1.774728116533986766, 42.31054587065082728, 4.000000000000000000 ) ) ;
#21404 = FACE_OUTER_BOUND ( 'NONE', #3846, .T. ) ;
#21405 = DIRECTION ( 'NONE',  ( 0.000000000000000000, -0.000000000000000000, 1.000000000000000000 ) ) ;
#21406 = EDGE_CURVE ( 'NONE', #21087, #12623, #12846, .T. ) ;
#21407 = ORIENTED_EDGE ( 'NONE', *, *, #18245, .F. ) ;
#21408 = DIRECTION ( 'NONE',  ( -0.000000000000000000, -0.000000000000000000, -1.000000000000000000 ) ) ;
#21409 = CIRCLE ( 'NONE', #10339, 1.999999999999991340 ) ;
#21410 = DIRECTION ( 'NONE',  ( 0.000000000000000000, 0.000000000000000000, 1.000000000000000000 ) ) ;
#21411 = ORIENTED_EDGE ( 'NONE', *, *, #17092, .F. ) ;
#21412 = ORIENTED_EDGE ( 'NONE', *, *, #11585, .T. ) ;
#21413 = FACE_OUTER_BOUND ( 'NONE', #11337, .T. ) ;
#21414 = EDGE_CURVE ( 'NONE', #21172, #12600, #4527, .T. ) ;
#21415 = ORIENTED_EDGE ( 'NONE', *, *, #7717, .F. ) ;
#21416 = CIRCLE ( 'NONE', #16391, 0.2999999999999999334 ) ;
#21417 = ORIENTED_EDGE ( 'NONE', *, *, #18273, .F. ) ;
#21418 = CIRCLE ( 'NONE', #2104, 1.299999999999999156 ) ;
#21419 = EDGE_CURVE ( 'NONE', #5585, #8010, #6829, .T. ) ;
#21420 = DIRECTION ( 'NONE',  ( 1.000000000000000000, 0.000000000000000000, 0.000000000000000000 ) ) ;
#21421 = ADVANCED_FACE ( 'NONE', ( #2861 ), #17951, .T. ) ;
#21422 = DIRECTION ( 'NONE',  ( 1.000000000000000000, 0.000000000000000000, 0.000000000000000000 ) ) ;
#21423 = ORIENTED_EDGE ( 'NONE', *, *, #15529, .T. ) ;
#21424 = EDGE_CURVE ( 'NONE', #11393, #10096, #5425, .T. ) ;
#21425 = FACE_OUTER_BOUND ( 'NONE', #5237, .T. ) ;
#21426 = AXIS2_PLACEMENT_3D ( 'NONE', #14243, #11416, #21840 ) ;
#21427 = CARTESIAN_POINT ( 'NONE',  ( 14.96174975910705918, 51.83053110199097091, 13.82013245744073160 ) ) ;
#21428 = CARTESIAN_POINT ( 'NONE',  ( -29.13662752439705272, 0.000000000000000000, 13.50000000000000000 ) ) ;
#21429 = CARTESIAN_POINT ( 'NONE',  ( -23.02398829872513630, 2.333754220862760409, 13.47170153661532943 ) ) ;
#21430 = VECTOR ( 'NONE', #9493, 1000.000000000000000 ) ;
#21431 = VERTEX_POINT ( 'NONE', #1160 ) ;
#21432 = DIRECTION ( 'NONE',  ( -0.000000000000000000, -0.000000000000000000, -1.000000000000000000 ) ) ;
#21433 = CARTESIAN_POINT ( 'NONE',  ( 17.45292532278785913, 0.000000000000000000, 68.50000000000000000 ) ) ;
#21434 = ORIENTED_EDGE ( 'NONE', *, *, #4528, .F. ) ;
#21435 = VERTEX_POINT ( 'NONE', #8006 ) ;
#21436 = EDGE_LOOP ( 'NONE', ( #6242, #20581, #5081, #13248 ) ) ;
#21437 = CYLINDRICAL_SURFACE ( 'NONE', #9568, 0.2999999999999999334 ) ;
#21438 = CARTESIAN_POINT ( 'NONE',  ( -32.50000000000002132, 71.00000000000001421, 3.200000000000000178 ) ) ;
#21439 = EDGE_CURVE ( 'NONE', #13135, #19461, #15284, .T. ) ;
#21440 = EDGE_LOOP ( 'NONE', ( #4637, #9422, #5711, #7697 ) ) ;
#21441 = CIRCLE ( 'NONE', #11766, 0.5000000000000004441 ) ;
#21442 = DIRECTION ( 'NONE',  ( 0.000000000000000000, -0.000000000000000000, 1.000000000000000000 ) ) ;
#21443 = CIRCLE ( 'NONE', #4276, 4.351418481279133665 ) ;
#21444 = CIRCLE ( 'NONE', #18219, 0.05000000000000143219 ) ;
#21445 = AXIS2_PLACEMENT_3D ( 'NONE', #3656, #9115, #14036 ) ;
#21446 = ORIENTED_EDGE ( 'NONE', *, *, #20612, .F. ) ;
#21447 = CARTESIAN_POINT ( 'NONE',  ( -9.718906393579157310, 40.01645089659919563, 70.88527860057354246 ) ) ;
#21448 =( BOUNDED_CURVE ( )  B_SPLINE_CURVE ( 3, ( #6205, #12773, #18033, #14570 ),
 .UNSPECIFIED., .F., .T. ) 
 B_SPLINE_CURVE_WITH_KNOTS ( ( 4, 4 ),
 ( 3.141592653589793116, 4.712388980384689674 ),
 .UNSPECIFIED. ) 
 CURVE ( )  GEOMETRIC_REPRESENTATION_ITEM ( )  RATIONAL_B_SPLINE_CURVE ( ( 1.000000000000000000, 0.8047378541243649375, 0.8047378541243649375, 1.000000000000000000 ) ) 
 REPRESENTATION_ITEM ( '' )  );
#21449 = DIRECTION ( 'NONE',  ( 0.000000000000000000, 0.000000000000000000, 1.000000000000000000 ) ) ;
#21450 = CARTESIAN_POINT ( 'NONE',  ( 0.000000000000000000, 42.31054587065082728, 49.71679706732589921 ) ) ;
#21451 = CARTESIAN_POINT ( 'NONE',  ( -10.22290649399594642, 41.92645089659918511, 68.06527860057354928 ) ) ;
#21452 = EDGE_CURVE ( 'NONE', #9043, #7172, #3227, .T. ) ;
#21453 = FACE_OUTER_BOUND ( 'NONE', #10990, .T. ) ;
#21454 = CARTESIAN_POINT ( 'NONE',  ( 33.19999999999999574, 85.00000000000000000, 78.79999999999999716 ) ) ;
#21455 = VERTEX_POINT ( 'NONE', #19859 ) ;
#21456 = CARTESIAN_POINT ( 'NONE',  ( -25.37540678000427263, -66.94634676501046044, 13.50000000000000000 ) ) ;
#21457 = ADVANCED_FACE ( 'NONE', ( #19522 ), #15716, .F. ) ;
#21458 = CARTESIAN_POINT ( 'NONE',  ( 29.13662752439705272, 4.700000000000000178, 3.500000000000000000 ) ) ;
#21459 = PLANE ( 'NONE',  #21947 ) ;
#21460 = CARTESIAN_POINT ( 'NONE',  ( -9.178906393579156386, 42.46645089659917716, 70.50000000000000000 ) ) ;
#21461 = ORIENTED_EDGE ( 'NONE', *, *, #1690, .F. ) ;
#21462 = CYLINDRICAL_SURFACE ( 'NONE', #15204, 0.5000000000000004441 ) ;
#21463 = DIRECTION ( 'NONE',  ( -1.000000000000000000, 0.000000000000000000, -0.000000000000000000 ) ) ;
#21464 =( REPRESENTATION_RELATIONSHIP ('NONE','NONE', #561, #10840 ) REPRESENTATION_RELATIONSHIP_WITH_TRANSFORMATION ( #21385 )SHAPE_REPRESENTATION_RELATIONSHIP( ) );
#21465 = CIRCLE ( 'NONE', #12495, 0.1000000000000028644 ) ;
#21466 = ORIENTED_EDGE ( 'NONE', *, *, #6310, .T. ) ;
#21467 = CIRCLE ( 'NONE', #2143, 2.881677036926254765 ) ;
#21468 = PRESENTATION_LAYER_ASSIGNMENT (  '', '', ( #1426 ) ) ;
#21469 = DIRECTION ( 'NONE',  ( 0.000000000000000000, 0.000000000000000000, 1.000000000000000000 ) ) ;
#21470 = CARTESIAN_POINT ( 'NONE',  ( 3.627054932750481964, -32.61873716947361856, 68.50000000000000000 ) ) ;
#21471 = ORIENTED_EDGE ( 'NONE', *, *, #18932, .F. ) ;
#21472 = VERTEX_POINT ( 'NONE', #7906 ) ;
#21473 = CARTESIAN_POINT ( 'NONE',  ( -15.16859876043988464, 52.00603549157913363, 13.50000000000000000 ) ) ;
#21474 = DIRECTION ( 'NONE',  ( -1.000000000000000000, -0.000000000000000000, -0.000000000000000000 ) ) ;
#21475 = ORIENTED_EDGE ( 'NONE', *, *, #8618, .T. ) ;
#21476 = EDGE_CURVE ( 'NONE', #16703, #17181, #7881, .T. ) ;
#21477 = EDGE_CURVE ( 'NONE', #5864, #4912, #3950, .T. ) ;
#21478 = EDGE_LOOP ( 'NONE', ( #6195, #15041, #6064, #15245 ) ) ;
#21479 = FACE_OUTER_BOUND ( 'NONE', #2235, .T. ) ;
#21480 = AXIS2_PLACEMENT_3D ( 'NONE', #18848, #10125, #20424 ) ;
#21481 = CARTESIAN_POINT ( 'NONE',  ( 29.13662752439705272, 0.000000000000000000, 13.50000000000000000 ) ) ;
#21482 = CARTESIAN_POINT ( 'NONE',  ( 34.39999999999998437, 85.00000000000000000, 0.6000000000000041966 ) ) ;
#21483 = CIRCLE ( 'NONE', #12513, 0.2999999999999999334 ) ;
#21484 = LINE ( 'NONE', #3645, #1306 ) ;
#21485 = DIRECTION ( 'NONE',  ( 0.000000000000000000, 0.000000000000000000, -1.000000000000000000 ) ) ;
#21486 = CYLINDRICAL_SURFACE ( 'NONE', #18661, 0.1000000000000028644 ) ;
#21487 = EDGE_CURVE ( 'NONE', #19966, #16243, #2736, .T. ) ;
#21488 = DIRECTION ( 'NONE',  ( 0.000000000000000000, 0.000000000000000000, 1.000000000000000000 ) ) ;
#21489 = CARTESIAN_POINT ( 'NONE',  ( -32.20000000000001705, -71.00000000000001421, 1.500000000000000000 ) ) ;
#21490 = CARTESIAN_POINT ( 'NONE',  ( 29.13662752439705272, 0.000000000000000000, -18.50000000000000000 ) ) ;
#21491 = ORIENTED_EDGE ( 'NONE', *, *, #2990, .F. ) ;
#21492 = CARTESIAN_POINT ( 'NONE',  ( -29.69597781366221767, 56.94165929845684815, 70.50000000000000000 ) ) ;
#21493 = DIRECTION ( 'NONE',  ( 1.000000000000000000, 0.000000000000000000, 0.000000000000000000 ) ) ;
#21494 = CARTESIAN_POINT ( 'NONE',  ( -1.774728116533986766, 42.36054587065083155, 43.70876104995653577 ) ) ;
#21495 = DIRECTION ( 'NONE',  ( 0.000000000000000000, 1.000000000000000000, -0.000000000000000000 ) ) ;
#21496 = DIRECTION ( 'NONE',  ( 0.000000000000000000, 0.000000000000000000, -1.000000000000000000 ) ) ;
#21497 = CIRCLE ( 'NONE', #43, 1.984122918275925462 ) ;
#21498 = ORIENTED_EDGE ( 'NONE', *, *, #16397, .T. ) ;
#21499 = ORIENTED_EDGE ( 'NONE', *, *, #16470, .T. ) ;
#21500 = CARTESIAN_POINT ( 'NONE',  ( 29.13662752439705272, 0.000000000000000000, 13.19999999999999929 ) ) ;
#21501 = ORIENTED_EDGE ( 'NONE', *, *, #14731, .T. ) ;
#21502 = ORIENTED_EDGE ( 'NONE', *, *, #18245, .T. ) ;
#21503 = EDGE_CURVE ( 'NONE', #3965, #14817, #6334, .T. ) ;
#21504 = AXIS2_PLACEMENT_3D ( 'NONE', #10563, #19076, #19502 ) ;
#21505 = DIRECTION ( 'NONE',  ( 1.000000000000000000, 0.000000000000000000, 0.000000000000000000 ) ) ;
#21506 = VERTEX_POINT ( 'NONE', #9792 ) ;
#21507 = PLANE ( 'NONE',  #4900 ) ;
#21508 = AXIS2_PLACEMENT_3D ( 'NONE', #11109, #15813, #2171 ) ;
#21509 = VERTEX_POINT ( 'NONE', #6006 ) ;
#21510 = FACE_OUTER_BOUND ( 'NONE', #6587, .T. ) ;
#21511 = CARTESIAN_POINT ( 'NONE',  ( 18.22752199202934520, -50.11873716947361856, 13.50000000000000000 ) ) ;
#21512 = FACE_OUTER_BOUND ( 'NONE', #11694, .T. ) ;
#21513 = AXIS2_PLACEMENT_3D ( 'NONE', #10483, #14042, #3883 ) ;
#21514 = LINE ( 'NONE', #4712, #15669 ) ;
#21515 = DIRECTION ( 'NONE',  ( -1.000000000000000000, 0.000000000000000000, 0.000000000000000000 ) ) ;
#21516 = DIRECTION ( 'NONE',  ( 1.734723475976806848E-16, 0.000000000000000000, -1.000000000000000000 ) ) ;
#21517 = AXIS2_PLACEMENT_3D ( 'NONE', #3974, #19399, #11001 ) ;
#21518 = CARTESIAN_POINT ( 'NONE',  ( 3.127054932750481964, 32.61873716947361856, 68.00000000000000000 ) ) ;
#21520 = ADVANCED_FACE ( 'NONE', ( #2623 ), #12671, .T. ) ;
#21519 = LINE ( 'NONE', #21077, #11243 ) ;
#21521 = AXIS2_PLACEMENT_3D ( 'NONE', #3862, #12324, #7329 ) ;
#21522 = ORIENTED_EDGE ( 'NONE', *, *, #6240, .F. ) ;
#21523 = FACE_OUTER_BOUND ( 'NONE', #18999, .T. ) ;
#21524 = AXIS2_PLACEMENT_3D ( 'NONE', #9440, #12892, #21650 ) ;
#21525 = DIRECTION ( 'NONE',  ( 1.000000000000000000, 0.000000000000000000, 0.000000000000000000 ) ) ;
#21526 = VERTEX_POINT ( 'NONE', #3523 ) ;
#21527 = ORIENTED_EDGE ( 'NONE', *, *, #2706, .F. ) ;
#21528 = DIRECTION ( 'NONE',  ( -1.000000000000000000, 0.000000000000000000, 0.000000000000000000 ) ) ;
#21529 = EDGE_CURVE ( 'NONE', #3217, #8345, #14294, .T. ) ;
#21530 = CARTESIAN_POINT ( 'NONE',  ( 0.000000000000000000, 0.000000000000000000, 0.000000000000000000 ) ) ;
#21531 = ADVANCED_FACE ( 'NONE', ( #15257 ), #2512, .T. ) ;
#21532 = ORIENTED_EDGE ( 'NONE', *, *, #14926, .F. ) ;
#21533 = ORIENTED_EDGE ( 'NONE', *, *, #14069, .T. ) ;
#21534 = VECTOR ( 'NONE', #19711, 1000.000000000000000 ) ;
#21535 = CARTESIAN_POINT ( 'NONE',  ( 15.14085429618050682, -52.10286008412593617, 13.87499998596578976 ) ) ;
#21536 = AXIS2_PLACEMENT_3D ( 'NONE', #13177, #16293, #7833 ) ;
#21537 = DIRECTION ( 'NONE',  ( 0.000000000000000000, 0.000000000000000000, 1.000000000000000000 ) ) ;
#21538 = ORIENTED_EDGE ( 'NONE', *, *, #13050, .F. ) ;
#21539 = LINE ( 'NONE', #1144, #2880 ) ;
#21540 = EDGE_CURVE ( 'NONE', #6536, #11776, #12510, .T. ) ;
#21541 = DIRECTION ( 'NONE',  ( 0.000000000000000000, 0.000000000000000000, -1.000000000000000000 ) ) ;
#21542 = FACE_OUTER_BOUND ( 'NONE', #3435, .T. ) ;
#21543 = DIRECTION ( 'NONE',  ( -1.224646799147353207E-16, -0.000000000000000000, -1.000000000000000000 ) ) ;
#21544 = ORIENTED_EDGE ( 'NONE', *, *, #17486, .T. ) ;
#21545 = FACE_OUTER_BOUND ( 'NONE', #12261, .T. ) ;
#21546 = DIRECTION ( 'NONE',  ( 2.107255972849994642E-16, 0.000000000000000000, 1.000000000000000000 ) ) ;
#21547 = ORIENTED_EDGE ( 'NONE', *, *, #11157, .T. ) ;
#21548 = ORIENTED_EDGE ( 'NONE', *, *, #3040, .F. ) ;
#21549 = ORIENTED_EDGE ( 'NONE', *, *, #586, .T. ) ;
#21550 = CARTESIAN_POINT ( 'NONE',  ( 15.21174975910707161, 51.61873716947361856, 68.00000000000000000 ) ) ;
#21551 = VECTOR ( 'NONE', #17659, 1000.000000000000000 ) ;
#21552 = CARTESIAN_POINT ( 'NONE',  ( 25.37540678000426908, 39.04634676501046187, 13.50000000000000000 ) ) ;
#21553 = ADVANCED_FACE ( 'NONE', ( #9901 ), #13354, .F. ) ;
#21554 = ORIENTED_EDGE ( 'NONE', *, *, #9815, .F. ) ;
#21555 = AXIS2_PLACEMENT_3D ( 'NONE', #3534, #10246, #13691 ) ;
#21556 = EDGE_CURVE ( 'NONE', #1513, #13945, #17871, .T. ) ;
#21557 = CARTESIAN_POINT ( 'NONE',  ( -13.37248138918699425, 42.46645089659917716, 70.50000000000000000 ) ) ;
#21558 = ORIENTED_EDGE ( 'NONE', *, *, #15899, .T. ) ;
#21559 = LINE ( 'NONE', #827, #18580 ) ;
#21560 = DIRECTION ( 'NONE',  ( 1.000000000000000000, 0.000000000000000000, 0.000000000000000000 ) ) ;
#21561 = VECTOR ( 'NONE', #3616, 1000.000000000000000 ) ;
#21562 = CARTESIAN_POINT ( 'NONE',  ( 1.774728116533979438, 42.36054587065083155, 27.80876104995653719 ) ) ;
#21563 = FACE_OUTER_BOUND ( 'NONE', #20131, .T. ) ;
#21564 = LINE ( 'NONE', #11355, #4704 ) ;
#21565 = LINE ( 'NONE', #4534, #16997 ) ;
#21566 = ORIENTED_EDGE ( 'NONE', *, *, #15707, .T. ) ;
#21567 = CARTESIAN_POINT ( 'NONE',  ( -3.627054932750481964, -32.11873716947361856, 68.00000000000000000 ) ) ;
#21568 = CARTESIAN_POINT ( 'NONE',  ( -14.96174975910705207, 41.81054587065082728, 13.79999999999999893 ) ) ;
#21569 = EDGE_CURVE ( 'NONE', #15018, #9891, #1087, .T. ) ;
#21570 = CARTESIAN_POINT ( 'NONE',  ( -1.724728116533986721, 42.36054587065083155, 45.76679706732590347 ) ) ;
#21571 = CARTESIAN_POINT ( 'NONE',  ( -4.603906393579157097, 42.46645089659918426, 74.06027860057353962 ) ) ;
#21572 = ORIENTED_EDGE ( 'NONE', *, *, #21424, .F. ) ;
#21573 = CARTESIAN_POINT ( 'NONE',  ( -30.67540678000428045, 0.000000000000000000, 3.799999999999999822 ) ) ;
#21574 = EDGE_LOOP ( 'NONE', ( #18629, #5142, #17787, #21980 ) ) ;
#21575 = DIRECTION ( 'NONE',  ( 1.000000000000000000, 0.000000000000000000, -0.000000000000000000 ) ) ;
#21576 = CARTESIAN_POINT ( 'NONE',  ( -23.02398829872513986, -2.157133568460768647, 13.19999999999999929 ) ) ;
#21577 = EDGE_LOOP ( 'NONE', ( #2349, #12816, #6821, #5846 ) ) ;
#21578 = ORIENTED_EDGE ( 'NONE', *, *, #10429, .T. ) ;
#21579 = ORIENTED_EDGE ( 'NONE', *, *, #15953, .T. ) ;
#21580 = CARTESIAN_POINT ( 'NONE',  ( -15.07123959906592248, 52.06981400416638905, 13.87294810141926149 ) ) ;
#21581 = EDGE_CURVE ( 'NONE', #7934, #818, #15372, .T. ) ;
#21582 = CARTESIAN_POINT ( 'NONE',  ( -17.45292532278785913, -34.11873716947361856, 68.50000000000000000 ) ) ;
#21583 = EDGE_CURVE ( 'NONE', #21328, #22135, #20096, .T. ) ;
#21584 =( BOUNDED_CURVE ( )  B_SPLINE_CURVE ( 3, ( #18211, #4446, #11588, #21916 ),
 .UNSPECIFIED., .F., .T. ) 
 B_SPLINE_CURVE_WITH_KNOTS ( ( 4, 4 ),
 ( 0.000000000000000000, 1.570796326794896558 ),
 .UNSPECIFIED. ) 
 CURVE ( )  GEOMETRIC_REPRESENTATION_ITEM ( )  RATIONAL_B_SPLINE_CURVE ( ( 1.000000000000000000, 0.8047378541243649375, 0.8047378541243649375, 1.000000000000000000 ) ) 
 REPRESENTATION_ITEM ( '' )  );
#21585 = VERTEX_POINT ( 'NONE', #16714 ) ;
#21586 = EDGE_CURVE ( 'NONE', #12600, #10704, #8242, .T. ) ;
#21587 = ORIENTED_EDGE ( 'NONE', *, *, #4705, .F. ) ;
#21588 = FACE_OUTER_BOUND ( 'NONE', #14852, .T. ) ;
#21589 = DIRECTION ( 'NONE',  ( -1.000000000000000000, 0.000000000000000000, -0.000000000000000000 ) ) ;
#21590 = CARTESIAN_POINT ( 'NONE',  ( -23.02398829872514696, -2.388551872609015359, 13.39771463486667358 ) ) ;
#21591 = DIRECTION ( 'NONE',  ( 0.000000000000000000, 0.000000000000000000, 1.000000000000000000 ) ) ;
#21592 = DIRECTION ( 'NONE',  ( -1.000000000000000000, 0.000000000000000000, 0.000000000000000000 ) ) ;
#21593 = FACE_OUTER_BOUND ( 'NONE', #14557, .T. ) ;
#21594 = ORIENTED_EDGE ( 'NONE', *, *, #21307, .T. ) ;
#21595 = DIRECTION ( 'NONE',  ( 8.673617379884034239E-17, 0.000000000000000000, -1.000000000000000000 ) ) ;
#21596 = DIRECTION ( 'NONE',  ( -1.000000000000000000, 0.000000000000000000, 0.000000000000000000 ) ) ;
#21597 = DIRECTION ( 'NONE',  ( -0.000000000000000000, -0.000000000000000000, 1.000000000000000000 ) ) ;
#21598 = COLOUR_RGB ( '', 0.09019608, 0.27058824, 0.51372549) ;
#21599 = ORIENTED_EDGE ( 'NONE', *, *, #6560, .T. ) ;
#21600 = CARTESIAN_POINT ( 'NONE',  ( -21.69312596654449621, 45.47506926072997402, 13.74999999999999822 ) ) ;
#21601 = EDGE_CURVE ( 'NONE', #19227, #1590, #19675, .T. ) ;
#21602 = LINE ( 'NONE', #9623, #15687 ) ;
#21603 = DIRECTION ( 'NONE',  ( 0.000000000000000000, 1.000000000000000000, 0.000000000000000000 ) ) ;
#21604 = ORIENTED_EDGE ( 'NONE', *, *, #20482, .F. ) ;
#21605 = CARTESIAN_POINT ( 'NONE',  ( -10.22290649399594642, 41.92645089659918511, 68.06527860057354928 ) ) ;
#21607 = AXIS2_PLACEMENT_3D ( 'NONE', #7583, #12683, #2635 ) ;
#21606 = FACE_OUTER_BOUND ( 'NONE', #1351, .T. ) ;
#21608 = ORIENTED_EDGE ( 'NONE', *, *, #15515, .F. ) ;
#21609 = ORIENTED_EDGE ( 'NONE', *, *, #2372, .F. ) ;
#21610 = FACE_OUTER_BOUND ( 'NONE', #1754, .T. ) ;
#21612 = EDGE_CURVE ( 'NONE', #2108, #13253, #12860, .T. ) ;
#21611 = ITEM_DEFINED_TRANSFORMATION ( 'NONE', 'NONE', #1209,  #17493 ) ;
#21613 = AXIS2_PLACEMENT_3D ( 'NONE', #7635, #5956, #7863 ) ;
#21614 = ORIENTED_EDGE ( 'NONE', *, *, #10331, .T. ) ;
#21615 = CARTESIAN_POINT ( 'NONE',  ( 15.21174975910705918, 41.81054587065082728, 13.75000000000000000 ) ) ;
#21616 = CARTESIAN_POINT ( 'NONE',  ( -35.00000000000001421, 85.00000000000000000, 80.00000000000000000 ) ) ;
#21617 = DIRECTION ( 'NONE',  ( -0.000000000000000000, 0.000000000000000000, 1.000000000000000000 ) ) ;
#21618 = LINE ( 'NONE', #16548, #16274 ) ;
#21619 = DIRECTION ( 'NONE',  ( 0.000000000000000000, 0.000000000000000000, -1.000000000000000000 ) ) ;
#21620 = CARTESIAN_POINT ( 'NONE',  ( 9.141460742840918030, -32.93424481021354921, 68.00000000000000000 ) ) ;
#21621 = ADVANCED_FACE ( 'NONE', ( #18619 ), #16802, .T. ) ;
#21622 = DIRECTION ( 'NONE',  ( 0.000000000000000000, 0.000000000000000000, 1.000000000000000000 ) ) ;
#21623 = CYLINDRICAL_SURFACE ( 'NONE', #14345, 0.04999999999999991257 ) ;
#21624 = EDGE_CURVE ( 'NONE', #7044, #9803, #13228, .T. ) ;
#21625 = CARTESIAN_POINT ( 'NONE',  ( 25.37540678000427263, -63.74634676501045050, 3.500000000000000000 ) ) ;
#21626 = AXIS2_PLACEMENT_3D ( 'NONE', #7992, #11549, #3387 ) ;
#21627 = VERTEX_POINT ( 'NONE', #18389 ) ;
#21628 = DIRECTION ( 'NONE',  ( 1.000000000000000000, 0.000000000000000000, 0.000000000000000000 ) ) ;
#21629 = PRODUCT_DEFINITION_SHAPE ( 'NONE', 'NONE',  #19421 ) ;
#21630 = DIRECTION ( 'NONE',  ( -1.000000000000000000, -0.000000000000000000, -4.336808689942194441E-15 ) ) ;
#21631 = VERTEX_POINT ( 'NONE', #8231 ) ;
#21632 = ORIENTED_EDGE ( 'NONE', *, *, #1464, .T. ) ;
#21633 = FACE_OUTER_BOUND ( 'NONE', #8822, .T. ) ;
#21634 = UNCERTAINTY_MEASURE_WITH_UNIT (LENGTH_MEASURE( 1.000000000000000082E-05 ), #17635, 'distance_accuracy_value', 'NONE');
#21635 = VERTEX_POINT ( 'NONE', #15042 ) ;
#21636 = EDGE_LOOP ( 'NONE', ( #3843, #10199, #9900, #10968 ) ) ;
#21637 = EDGE_CURVE ( 'NONE', #19513, #712, #13598, .T. ) ;
#21638 = AXIS2_PLACEMENT_3D ( 'NONE', #1559, #21847, #9859 ) ;
#21639 = AXIS2_PLACEMENT_3D ( 'NONE', #15310, #11827, #16760 ) ;
#21640 = ORIENTED_EDGE ( 'NONE', *, *, #1435, .F. ) ;
#21641 = CARTESIAN_POINT ( 'NONE',  ( 0.000000000000000000, 0.000000000000000000, 7.500000000000000000 ) ) ;
#21642 = CARTESIAN_POINT ( 'NONE',  ( 1.724728116533979616, 43.31054587065082728, 35.75876104995654003 ) ) ;
#21643 = ORIENTED_EDGE ( 'NONE', *, *, #12737, .F. ) ;
#21644 =( LENGTH_UNIT ( ) NAMED_UNIT ( * ) SI_UNIT ( .MILLI., .METRE. ) );
#21645 = EDGE_CURVE ( 'NONE', #2851, #5528, #18235, .T. ) ;
#21646 = CARTESIAN_POINT ( 'NONE',  ( 9.641460742840918030, -32.61873716947361856, 68.00000000000000000 ) ) ;
#21647 = CARTESIAN_POINT ( 'NONE',  ( 3.127054932750481964, 32.61873716947361856, 68.00000000000000000 ) ) ;
#21648 = CYLINDRICAL_SURFACE ( 'NONE', #15911, 0.5000000000000000000 ) ;
#21649 = ORIENTED_EDGE ( 'NONE', *, *, #8718, .F. ) ;
#21650 = DIRECTION ( 'NONE',  ( 0.000000000000000000, 0.000000000000000000, -1.000000000000000000 ) ) ;
#21651 = ORIENTED_EDGE ( 'NONE', *, *, #16660, .F. ) ;
#21652 = VERTEX_POINT ( 'NONE', #13469 ) ;
#21653 = VECTOR ( 'NONE', #20542, 1000.000000000000000 ) ;
#21654 = EDGE_LOOP ( 'NONE', ( #20589, #11997, #8094, #7490 ) ) ;
#21655 = DIRECTION ( 'NONE',  ( 1.000000000000000000, 0.000000000000000000, -2.388292521039847891E-16 ) ) ;
#21656 = LINE ( 'NONE', #6326, #10328 ) ;
#21657 = EDGE_LOOP ( 'NONE', ( #15475, #6603, #19112, #8362, #16904, #12562 ) ) ;
#21658 = CARTESIAN_POINT ( 'NONE',  ( -25.37540678000427263, 63.74634676501045050, 7.500000000000000000 ) ) ;
#21659 = EDGE_CURVE ( 'NONE', #18309, #8904, #10392, .T. ) ;
#21660 = ORIENTED_EDGE ( 'NONE', *, *, #15226, .F. ) ;
#21661 = DIRECTION ( 'NONE',  ( 2.107255972849994642E-16, -0.000000000000000000, 1.000000000000000000 ) ) ;
#21662 = CARTESIAN_POINT ( 'NONE',  ( -1.824728116533986810, 42.36054587065083155, 37.71679706732590631 ) ) ;
#21663 = CARTESIAN_POINT ( 'NONE',  ( -30.37540678000427619, 6.000000000000000000, 3.499999999999999556 ) ) ;
#21664 = AXIS2_PLACEMENT_3D ( 'NONE', #5849, #14324, #17794 ) ;
#21665 = AXIS2_PLACEMENT_3D ( 'NONE', #7771, #6101, #2610 ) ;
#21666 = DIRECTION ( 'NONE',  ( 0.000000000000000000, 0.000000000000000000, -1.000000000000000000 ) ) ;
#21667 = AXIS2_PLACEMENT_3D ( 'NONE', #17601, #2379, #10679 ) ;
#21668 = EDGE_LOOP ( 'NONE', ( #12615, #17009, #16203, #16512 ) ) ;
#21669 = CARTESIAN_POINT ( 'NONE',  ( 15.21174975910707161, -51.61873716947361856, 68.00000000000000000 ) ) ;
#21670 = CARTESIAN_POINT ( 'NONE',  ( 1.724728116533979838, 42.36054587065083155, 45.66679706732590205 ) ) ;
#21671 = EDGE_CURVE ( 'NONE', #16763, #6333, #8440, .T. ) ;
#21672 = ADVANCED_FACE ( 'NONE', ( #47 ), #19374, .T. ) ;
#21673 = EDGE_CURVE ( 'NONE', #17663, #7349, #8956, .T. ) ;
#21674 = DIRECTION ( 'NONE',  ( -0.000000000000000000, -1.000000000000000000, -0.000000000000000000 ) ) ;
#21675 = CARTESIAN_POINT ( 'NONE',  ( -29.69597781366221767, 58.69165929845684815, 68.75000000000000000 ) ) ;
#21676 = ORIENTED_EDGE ( 'NONE', *, *, #18492, .F. ) ;
#21677 = LINE ( 'NONE', #16056, #4480 ) ;
#21678 = CARTESIAN_POINT ( 'NONE',  ( 1.724728116533979838, 43.26054587065083012, 49.66679706732590915 ) ) ;
#21679 = VERTEX_POINT ( 'NONE', #4145 ) ;
#21680 = CARTESIAN_POINT ( 'NONE',  ( -1.724728116533986721, 42.36054587065083155, 43.70876104995653577 ) ) ;
#21681 = CARTESIAN_POINT ( 'NONE',  ( 28.57540678000427548, 63.74634676501045050, 13.50000000000000000 ) ) ;
#21682 = ORIENTED_EDGE ( 'NONE', *, *, #19935, .F. ) ;
#21683 = VECTOR ( 'NONE', #18959, 1000.000000000000000 ) ;
#21684 = VERTEX_POINT ( 'NONE', #14322 ) ;
#21685 = CIRCLE ( 'NONE', #5252, 0.5999999999999999778 ) ;
#21686 = VERTEX_POINT ( 'NONE', #12523 ) ;
#21687 = CARTESIAN_POINT ( 'NONE',  ( -15.05373532783226054, 52.39333378048836920, 13.50000000000000000 ) ) ;
#21688 = DIRECTION ( 'NONE',  ( 1.000000000000000000, 0.000000000000000000, 0.000000000000000000 ) ) ;
#21689 = VERTEX_POINT ( 'NONE', #146 ) ;
#21690 = VECTOR ( 'NONE', #20428, 1000.000000000000000 ) ;
#21691 = EDGE_CURVE ( 'NONE', #3263, #12488, #21829, .T. ) ;
#21692 = ORIENTED_EDGE ( 'NONE', *, *, #8127, .T. ) ;
#21693 = CARTESIAN_POINT ( 'NONE',  ( 3.627054932750481964, 33.43424481021354921, 68.00000000000000000 ) ) ;
#21694 = CARTESIAN_POINT ( 'NONE',  ( 0.000000000000000000, 51.61873716947361856, 14.00000000000000000 ) ) ;
#21695 = LINE ( 'NONE', #7831, #16701 ) ;
#21696 = VECTOR ( 'NONE', #8122, 1000.000000000000000 ) ;
#21697 = CIRCLE ( 'NONE', #10601, 0.2999999999999999334 ) ;
#21698 = CARTESIAN_POINT ( 'NONE',  ( -14.71174975910705029, 51.86873716947361856, 68.00000000000000000 ) ) ;
#21699 = AXIS2_PLACEMENT_3D ( 'NONE', #16860, #20225, #4898 ) ;
#21700 = DIRECTION ( 'NONE',  ( 0.000000000000000000, -1.000000000000000000, 0.000000000000000000 ) ) ;
#21701 = PLANE ( 'NONE',  #270 ) ;
#21702 = EDGE_CURVE ( 'NONE', #6237, #13366, #21176, .T. ) ;
#21703 = EDGE_CURVE ( 'NONE', #9296, #1345, #11182, .T. ) ;
#21704 = CARTESIAN_POINT ( 'NONE',  ( -30.07540678000427548, 63.74634676501045050, 7.500000000000000000 ) ) ;
#21705 = ORIENTED_EDGE ( 'NONE', *, *, #22130, .F. ) ;
#21706 = CARTESIAN_POINT ( 'NONE',  ( -15.95292532278785913, 52.11873716947361856, 14.00000000000000000 ) ) ;
#21707 = VECTOR ( 'NONE', #11442, 1000.000000000000000 ) ;
#21708 = EDGE_CURVE ( 'NONE', #4042, #847, #16074, .T. ) ;
#21709 = CARTESIAN_POINT ( 'NONE',  ( -25.37540678000426908, 36.74634676501047181, 13.79999999999999893 ) ) ;
#21710 = ORIENTED_EDGE ( 'NONE', *, *, #20467, .F. ) ;
#21711 = CARTESIAN_POINT ( 'NONE',  ( -15.95292532278785913, 34.11873716947361856, 109.6002446535588319 ) ) ;
#21712 = DIRECTION ( 'NONE',  ( 0.000000000000000000, -0.000000000000000000, 1.000000000000000000 ) ) ;
#21713 = ORIENTED_EDGE ( 'NONE', *, *, #16694, .T. ) ;
#21714 = AXIS2_PLACEMENT_3D ( 'NONE', #3497, #20510, #6546 ) ;
#21715 = AXIS2_PLACEMENT_3D ( 'NONE', #16888, #20486, #3584 ) ;
#21716 = ORIENTED_EDGE ( 'NONE', *, *, #606, .T. ) ;
#21717 = CARTESIAN_POINT ( 'NONE',  ( 0.000000000000000000, 32.61873716947361856, 68.00000000000000000 ) ) ;
#21718 = EDGE_CURVE ( 'NONE', #12330, #7824, #21064, .T. ) ;
#21719 = VECTOR ( 'NONE', #5192, 1000.000000000000000 ) ;
#21720 = ORIENTED_EDGE ( 'NONE', *, *, #5842, .F. ) ;
#21721 = EDGE_CURVE ( 'NONE', #21652, #16241, #9299, .T. ) ;
#21722 = AXIS2_PLACEMENT_3D ( 'NONE', #12180, #19035, #16067 ) ;
#21723 = EDGE_CURVE ( 'NONE', #9996, #21689, #6843, .T. ) ;
#21724 = DIRECTION ( 'NONE',  ( 0.000000000000000000, 0.000000000000000000, 1.000000000000000000 ) ) ;
#21725 = LINE ( 'NONE', #4809, #12380 ) ;
#21726 = CARTESIAN_POINT ( 'NONE',  ( -30.67540678000428045, 63.74634676501045050, 3.799999999999999822 ) ) ;
#21727 = DIRECTION ( 'NONE',  ( 0.000000000000000000, 0.000000000000000000, 1.000000000000000000 ) ) ;
#21728 = AXIS2_PLACEMENT_3D ( 'NONE', #19443, #14396, #7270 ) ;
#21729 = VECTOR ( 'NONE', #12270, 1000.000000000000000 ) ;
#21730 = VECTOR ( 'NONE', #17994, 1000.000000000000000 ) ;
#21731 = CARTESIAN_POINT ( 'NONE',  ( -9.718906393579157310, 41.66638367286108746, 68.06527860057354928 ) ) ;
#21732 = CARTESIAN_POINT ( 'NONE',  ( 8.641460742840918030, -33.43424481021354921, 68.50000000000000000 ) ) ;
#21733 = EDGE_CURVE ( 'NONE', #183, #16035, #4372, .T. ) ;
#21734 = LINE ( 'NONE', #4609, #12577 ) ;
#21735 = AXIS2_PLACEMENT_3D ( 'NONE', #5682, #7133, #12344 ) ;
#21736 = LINE ( 'NONE', #2925, #10440 ) ;
#21737 = DIRECTION ( 'NONE',  ( 1.000000000000000000, 0.000000000000000000, 0.000000000000000000 ) ) ;
#21738 = AXIS2_PLACEMENT_3D ( 'NONE', #7664, #1258, #13128 ) ;
#21739 = AXIS2_PLACEMENT_3D ( 'NONE', #5347, #3877, #20879 ) ;
#21740 = DIRECTION ( 'NONE',  ( 1.000000000000000000, 0.000000000000000000, 0.000000000000000000 ) ) ;
#21741 = ORIENTED_EDGE ( 'NONE', *, *, #8597, .F. ) ;
#21742 = DIRECTION ( 'NONE',  ( -0.000000000000000000, -0.000000000000000000, 1.000000000000000000 ) ) ;
#21743 = CARTESIAN_POINT ( 'NONE',  ( -29.69597781366221767, 58.94165929845684815, 68.75000000000000000 ) ) ;
#21744 = ORIENTED_EDGE ( 'NONE', *, *, #17317, .T. ) ;
#21745 = ORIENTED_EDGE ( 'NONE', *, *, #20712, .T. ) ;
#21746 = CARTESIAN_POINT ( 'NONE',  ( 29.69597781366221767, 58.94165929845684104, 70.25000000000000000 ) ) ;
#21747 = TOROIDAL_SURFACE ( 'NONE', #3159, 0.05000000000000000278, 0.05000000000000000278 ) ;
#21748 = CIRCLE ( 'NONE', #14559, 0.04999999999999991257 ) ;
#21749 = ADVANCED_FACE ( 'NONE', ( #2350 ), #15388, .T. ) ;
#21750 = ORIENTED_EDGE ( 'NONE', *, *, #7127, .T. ) ;
#21751 = ADVANCED_FACE ( 'NONE', ( #21391 ), #9184, .T. ) ;
#21752 = AXIS2_PLACEMENT_3D ( 'NONE', #18794, #13643, #13415 ) ;
#21753 = VECTOR ( 'NONE', #7539, 1000.000000000000000 ) ;
#21754 = EDGE_LOOP ( 'NONE', ( #17598, #10344, #17516, #11919 ) ) ;
#21755 = VECTOR ( 'NONE', #12081, 1000.000000000000000 ) ;
#21756 = CARTESIAN_POINT ( 'NONE',  ( -14.66174975910705136, -51.76873716947361714, 13.50000000000000000 ) ) ;
#21757 = CARTESIAN_POINT ( 'NONE',  ( -32.20000000000001705, 71.00000000000001421, 1.500000000000000000 ) ) ;
#21758 = EDGE_LOOP ( 'NONE', ( #15955, #5480, #13847, #17996 ) ) ;
#21759 = DIRECTION ( 'NONE',  ( 0.000000000000000000, -1.000000000000000000, 0.000000000000000000 ) ) ;
#21760 = DIRECTION ( 'NONE',  ( -0.000000000000000000, -1.000000000000000000, -0.000000000000000000 ) ) ;
#21761 = VECTOR ( 'NONE', #7948, 1000.000000000000000 ) ;
#21762 = CARTESIAN_POINT ( 'NONE',  ( -17.95292532278785913, 0.000000000000000000, 42.50000000000000711 ) ) ;
#21763 = LINE ( 'NONE', #4404, #15753 ) ;
#21764 = CIRCLE ( 'NONE', #17811, 0.05000000000000143219 ) ;
#21765 = ORIENTED_EDGE ( 'NONE', *, *, #1563, .F. ) ;
#21766 = VECTOR ( 'NONE', #3961, 1000.000000000000000 ) ;
#21767 = ORIENTED_EDGE ( 'NONE', *, *, #16636, .F. ) ;
#21768 = VERTEX_POINT ( 'NONE', #20645 ) ;
#21769 = DIRECTION ( 'NONE',  ( 1.000000000000000000, 0.000000000000000000, 6.123233995736764803E-17 ) ) ;
#21770 = CIRCLE ( 'NONE', #20700, 0.2500000000000002220 ) ;
#21771 = DIRECTION ( 'NONE',  ( 0.000000000000000000, 0.000000000000000000, 1.000000000000000000 ) ) ;
#21772 = ORIENTED_EDGE ( 'NONE', *, *, #504, .T. ) ;
#21773 = CARTESIAN_POINT ( 'NONE',  ( -10.48680304830625154, -2.489116863435002713, 68.50000000000000000 ) ) ;
#21774 = EDGE_CURVE ( 'NONE', #14314, #16813, #11085, .T. ) ;
#21775 = VECTOR ( 'NONE', #10363, 1000.000000000000000 ) ;
#21776 = ORIENTED_EDGE ( 'NONE', *, *, #1832, .F. ) ;
#21777 = DIRECTION ( 'NONE',  ( -0.000000000000000000, 0.000000000000000000, 1.000000000000000000 ) ) ;
#21778 = EDGE_CURVE ( 'NONE', #17444, #11974, #12628, .T. ) ;
#21779 = VECTOR ( 'NONE', #404, 1000.000000000000000 ) ;
#21780 = DIRECTION ( 'NONE',  ( 1.000000000000000000, 0.000000000000000000, -0.000000000000000000 ) ) ;
#21781 = FACE_OUTER_BOUND ( 'NONE', #248, .T. ) ;
#21782 = AXIS2_PLACEMENT_3D ( 'NONE', #12120, #260, #20864 ) ;
#21783 = CARTESIAN_POINT ( 'NONE',  ( 1.724728116533979838, 42.31054587065082728, 37.66679706732590915 ) ) ;
#21784 = ORIENTED_EDGE ( 'NONE', *, *, #21145, .T. ) ;
#21785 = DIRECTION ( 'NONE',  ( 0.000000000000000000, -1.000000000000000000, 0.000000000000000000 ) ) ;
#21786 = FACE_OUTER_BOUND ( 'NONE', #11449, .T. ) ;
#21787 = AXIS2_PLACEMENT_3D ( 'NONE', #7841, #6053, #21493 ) ;
#21788 = FACE_OUTER_BOUND ( 'NONE', #16884, .T. ) ;
#21789 = CARTESIAN_POINT ( 'NONE',  ( 3.127054932750481964, -32.93424481021354921, 68.50000000000000000 ) ) ;
#21790 = ORIENTED_EDGE ( 'NONE', *, *, #3092, .T. ) ;
#21791 = CARTESIAN_POINT ( 'NONE',  ( -14.96174975910705207, 50.19799549595485644, -3.500000000000003109 ) ) ;
#21792 = DIRECTION ( 'NONE',  ( 0.000000000000000000, 1.000000000000000000, 0.000000000000000000 ) ) ;
#21793 = DIRECTION ( 'NONE',  ( 0.000000000000000000, 0.000000000000000000, 1.000000000000000000 ) ) ;
#21794 = ORIENTED_EDGE ( 'NONE', *, *, #6604, .T. ) ;
#21795 = CARTESIAN_POINT ( 'NONE',  ( 0.000000000000000000, -38.74634676501045760, 42.50000000000000000 ) ) ;
#21796 = DIRECTION ( 'NONE',  ( 0.000000000000000000, 1.000000000000000000, 0.000000000000000000 ) ) ;
#21797 = EDGE_CURVE ( 'NONE', #6000, #6081, #673, .T. ) ;
#21798 = ORIENTED_EDGE ( 'NONE', *, *, #14641, .T. ) ;
#21799 = ORIENTED_EDGE ( 'NONE', *, *, #18101, .T. ) ;
#21800 = ORIENTED_EDGE ( 'NONE', *, *, #18910, .F. ) ;
#21801 = CARTESIAN_POINT ( 'NONE',  ( -18.22752199202934520, 39.04634676501046187, 13.50000000000000000 ) ) ;
#21802 = CARTESIAN_POINT ( 'NONE',  ( 30.67540678000427690, 6.000000000000000000, 3.500000000000000000 ) ) ;
#21803 = AXIS2_PLACEMENT_3D ( 'NONE', #1625, #9927, #10144 ) ;
#21804 = ORIENTED_EDGE ( 'NONE', *, *, #21832, .F. ) ;
#21805 = EDGE_CURVE ( 'NONE', #15362, #5205, #18963, .T. ) ;
#21806 = EDGE_CURVE ( 'NONE', #2890, #15663, #2878, .T. ) ;
#21807 = EDGE_LOOP ( 'NONE', ( #2282, #10605, #314, #11613, #6967, #16581, #22142, #7955 ) ) ;
#21808 = DIRECTION ( 'NONE',  ( -1.000000000000000000, 0.000000000000000000, -0.000000000000000000 ) ) ;
#21809 = CARTESIAN_POINT ( 'NONE',  ( 17.45292532278785913, 0.000000000000000000, 68.50000000000000000 ) ) ;
#21810 = CARTESIAN_POINT ( 'NONE',  ( -23.04273156199908712, -2.261510999193106386, 13.20000000000004015 ) ) ;
#21811 = FACE_OUTER_BOUND ( 'NONE', #15868, .T. ) ;
#21812 = CARTESIAN_POINT ( 'NONE',  ( 8.641460742840918030, 33.43424481021354921, 42.50000000000000000 ) ) ;
#21813 = DIRECTION ( 'NONE',  ( 1.000000000000000000, 0.000000000000000000, 0.000000000000000000 ) ) ;
#21814 = DIRECTION ( 'NONE',  ( 0.000000000000000000, 1.000000000000000000, 0.000000000000000000 ) ) ;
#21815 = VECTOR ( 'NONE', #15697, 1000.000000000000000 ) ;
#21816 = AXIS2_PLACEMENT_3D ( 'NONE', #2071, #5558, #279 ) ;
#21817 = LINE ( 'NONE', #15180, #6352 ) ;
#21818 = DIRECTION ( 'NONE',  ( 0.000000000000000000, 1.000000000000000000, 0.000000000000000000 ) ) ;
#21819 = ORIENTED_EDGE ( 'NONE', *, *, #3347, .F. ) ;
#21820 = DIRECTION ( 'NONE',  ( -1.000000000000000000, -0.000000000000000000, -0.000000000000000000 ) ) ;
#21821 = EDGE_CURVE ( 'NONE', #4141, #10497, #18595, .T. ) ;
#21822 = DIRECTION ( 'NONE',  ( -0.000000000000000000, -1.000000000000000000, -0.000000000000000000 ) ) ;
#21823 = VERTEX_POINT ( 'NONE', #16335 ) ;
#21824 = DIRECTION ( 'NONE',  ( -2.832483164223434527E-16, -1.000000000000000000, 0.000000000000000000 ) ) ;
#21825 = CARTESIAN_POINT ( 'NONE',  ( 1.824728116533979261, 42.36054587065083155, 35.80876104995653009 ) ) ;
#21826 = ORIENTED_EDGE ( 'NONE', *, *, #880, .F. ) ;
#21827 = ORIENTED_EDGE ( 'NONE', *, *, #17758, .T. ) ;
#21828 = FACE_OUTER_BOUND ( 'NONE', #20834, .T. ) ;
#21829 = CIRCLE ( 'NONE', #20753, 4.999999999999997335 ) ;
#21830 = ADVANCED_FACE ( 'NONE', ( #2255 ), #14657, .F. ) ;
#21831 = AXIS2_PLACEMENT_3D ( 'NONE', #3949, #19152, #2357 ) ;
#21832 = EDGE_CURVE ( 'NONE', #9400, #1945, #17531, .T. ) ;
#21833 = EDGE_LOOP ( 'NONE', ( #20166, #9990, #8221, #7602 ) ) ;
#21834 = ADVANCED_FACE ( 'NONE', ( #14431, #9417, #16216, #9087, #10771, #893, #17683, #7742 ), #10872, .T. ) ;
#21835 = DIRECTION ( 'NONE',  ( -1.000000000000000000, 0.000000000000000000, 0.000000000000000000 ) ) ;
#21836 = ORIENTED_EDGE ( 'NONE', *, *, #19475, .F. ) ;
#21837 = DIRECTION ( 'NONE',  ( -0.000000000000000000, -0.000000000000000000, -1.000000000000000000 ) ) ;
#21838 = CARTESIAN_POINT ( 'NONE',  ( -1.724728116533986721, 42.31054587065082728, 39.75876104995654003 ) ) ;
#21839 = DIRECTION ( 'NONE',  ( -0.000000000000000000, 1.000000000000000000, -0.000000000000000000 ) ) ;
#21840 = DIRECTION ( 'NONE',  ( -1.000000000000000000, 0.000000000000000000, 0.000000000000000000 ) ) ;
#21841 = CARTESIAN_POINT ( 'NONE',  ( -29.37540678000427619, 4.700000000000000178, 3.500000000000000000 ) ) ;
#21842 = AXIS2_PLACEMENT_3D ( 'NONE', #11244, #14821, #2639 ) ;
#21843 = EDGE_CURVE ( 'NONE', #12849, #19512, #4680, .T. ) ;
#21844 = AXIS2_PLACEMENT_3D ( 'NONE', #9719, #14956, #2769 ) ;
#21845 = CYLINDRICAL_SURFACE ( 'NONE', #10867, 0.1000000000000028644 ) ;
#21846 = CARTESIAN_POINT ( 'NONE',  ( -9.178906393579158163, 42.46645089659918426, 68.06527860057354928 ) ) ;
#21847 = DIRECTION ( 'NONE',  ( -0.000000000000000000, -0.000000000000000000, -1.000000000000000000 ) ) ;
#21848 = ORIENTED_EDGE ( 'NONE', *, *, #14831, .F. ) ;
#21849 = DIRECTION ( 'NONE',  ( -0.000000000000000000, 0.000000000000000000, 1.000000000000000000 ) ) ;
#21850 = EDGE_LOOP ( 'NONE', ( #19984, #14893, #644, #1548 ) ) ;
#21851 = DIRECTION ( 'NONE',  ( 0.000000000000000000, 0.000000000000000000, 1.000000000000000000 ) ) ;
#21852 = DIRECTION ( 'NONE',  ( 0.000000000000000000, -0.000000000000000000, -1.000000000000000000 ) ) ;
#21853 = ORIENTED_EDGE ( 'NONE', *, *, #17756, .F. ) ;
#21854 = EDGE_LOOP ( 'NONE', ( #20454, #2942, #16794, #11138 ) ) ;
#21855 = DIRECTION ( 'NONE',  ( 1.000000000000000000, 0.000000000000000000, 0.000000000000000000 ) ) ;
#21856 = ORIENTED_EDGE ( 'NONE', *, *, #2791, .F. ) ;
#21857 = CIRCLE ( 'NONE', #17557, 0.5000000000000004441 ) ;
#21858 = EDGE_CURVE ( 'NONE', #1401, #17690, #19602, .T. ) ;
#21859 = ORIENTED_EDGE ( 'NONE', *, *, #16950, .T. ) ;
#21860 = ADVANCED_FACE ( 'NONE', ( #5856 ), #21078, .F. ) ;
#21861 = ORIENTED_EDGE ( 'NONE', *, *, #20245, .F. ) ;
#21862 = ORIENTED_EDGE ( 'NONE', *, *, #14276, .T. ) ;
#21863 = DIRECTION ( 'NONE',  ( -2.107255972849994642E-16, 0.000000000000000000, -1.000000000000000000 ) ) ;
#21864 = CIRCLE ( 'NONE', #14699, 0.5000000000000004441 ) ;
#21865 = DIRECTION ( 'NONE',  ( 0.000000000000000000, -0.000000000000000000, -1.000000000000000000 ) ) ;
#21866 = VERTEX_POINT ( 'NONE', #19713 ) ;
#21867 = CARTESIAN_POINT ( 'NONE',  ( -30.79999999999999361, -84.70000000000001705, 1.199999999999999734 ) ) ;
#21868 = VECTOR ( 'NONE', #10444, 1000.000000000000000 ) ;
#21869 = CARTESIAN_POINT ( 'NONE',  ( -23.02398829872513986, 3.528912754968630772, 13.79999999999999893 ) ) ;
#21870 = VECTOR ( 'NONE', #4847, 1000.000000000000000 ) ;
#21871 = CARTESIAN_POINT ( 'NONE',  ( 1.724728116533979616, 42.36054587065083155, 27.80876104995653719 ) ) ;
#21872 = DIRECTION ( 'NONE',  ( 0.000000000000000000, 1.000000000000000000, 0.000000000000000000 ) ) ;
#21873 = EDGE_CURVE ( 'NONE', #3158, #15670, #5756, .T. ) ;
#21874 = ORIENTED_EDGE ( 'NONE', *, *, #5406, .F. ) ;
#21875 = CARTESIAN_POINT ( 'NONE',  ( 17.93704824106378837, 0.000000000000000000, 13.87500000000000000 ) ) ;
#21876 = ORIENTED_EDGE ( 'NONE', *, *, #6480, .F. ) ;
#21877 = VERTEX_POINT ( 'NONE', #685 ) ;
#21878 = VERTEX_POINT ( 'NONE', #7536 ) ;
#21879 = CARTESIAN_POINT ( 'NONE',  ( 0.000000000000000000, 52.11873716947361856, 68.00000000000000000 ) ) ;
#21880 = DIRECTION ( 'NONE',  ( 1.000000000000000000, 0.000000000000000000, -0.000000000000000000 ) ) ;
#21881 = ORIENTED_EDGE ( 'NONE', *, *, #7228, .T. ) ;
#21882 = CIRCLE ( 'NONE', #19727, 0.3000000000000003775 ) ;
#21883 = CARTESIAN_POINT ( 'NONE',  ( -25.37540678000429040, -36.74634676501047181, 13.79999999999999893 ) ) ;
#21884 = EDGE_CURVE ( 'NONE', #10960, #17196, #4157, .T. ) ;
#21885 = AXIS2_PLACEMENT_3D ( 'NONE', #3607, #9297, #18005 ) ;
#21886 = AXIS2_PLACEMENT_3D ( 'NONE', #11495, #6155, #18323 ) ;
#21887 = ORIENTED_EDGE ( 'NONE', *, *, #7683, .T. ) ;
#21888 = DIRECTION ( 'NONE',  ( 0.000000000000000000, 0.000000000000000000, 1.000000000000000000 ) ) ;
#21889 = CARTESIAN_POINT ( 'NONE',  ( 1.774728116533979883, 43.26054587065083012, 45.66679706732590205 ) ) ;
#21890 = CARTESIAN_POINT ( 'NONE',  ( 29.37540678000427619, -5.000000000000000000, 7.500000000000000000 ) ) ;
#21891 = CARTESIAN_POINT ( 'NONE',  ( -1.824728116533986810, 42.36054587065083155, 31.80876104995653719 ) ) ;
#21892 = EDGE_LOOP ( 'NONE', ( #6161, #1184, #20007, #15346 ) ) ;
#21893 = DIRECTION ( 'NONE',  ( 0.000000000000000000, 0.000000000000000000, -1.000000000000000000 ) ) ;
#21894 = CARTESIAN_POINT ( 'NONE',  ( 32.20000000000001705, -71.00000000000001421, 1.500000000000000000 ) ) ;
#21895 = DIRECTION ( 'NONE',  ( -0.000000000000000000, -1.000000000000000000, -0.000000000000000000 ) ) ;
#21896 = DIRECTION ( 'NONE',  ( -0.000000000000000000, 1.000000000000000000, 0.000000000000000000 ) ) ;
#21897 = ORIENTED_EDGE ( 'NONE', *, *, #6389, .T. ) ;
#21898 = CARTESIAN_POINT ( 'NONE',  ( 25.37540678000427263, -68.74634676501045760, 7.500000000000000000 ) ) ;
#21899 = EDGE_CURVE ( 'NONE', #2296, #14801, #12636, .T. ) ;
#21900 = ORIENTED_EDGE ( 'NONE', *, *, #5816, .F. ) ;
#21901 = PLANE ( 'NONE',  #11619 ) ;
#21902 = CIRCLE ( 'NONE', #2592, 0.5000000000000004441 ) ;
#21903 = DIRECTION ( 'NONE',  ( 0.000000000000000000, 1.000000000000000000, -0.000000000000000000 ) ) ;
#21904 = ADVANCED_FACE ( 'NONE', ( #2534 ), #19879, .T. ) ;
#21905 = ORIENTED_EDGE ( 'NONE', *, *, #7447, .T. ) ;
#21906 = ORIENTED_EDGE ( 'NONE', *, *, #14383, .F. ) ;
#21907 = ORIENTED_EDGE ( 'NONE', *, *, #17405, .F. ) ;
#21908 = CARTESIAN_POINT ( 'NONE',  ( -14.75141515765153954, 52.14252004795846318, 13.50000000000000000 ) ) ;
#21909 = FACE_OUTER_BOUND ( 'NONE', #6757, .T. ) ;
#21910 = ORIENTED_EDGE ( 'NONE', *, *, #10143, .F. ) ;
#21911 = DIRECTION ( 'NONE',  ( 0.000000000000000000, 0.000000000000000000, 1.000000000000000000 ) ) ;
#21912 = CIRCLE ( 'NONE', #9746, 0.2500000000000002220 ) ;
#21913 = ORIENTED_EDGE ( 'NONE', *, *, #11020, .T. ) ;
#21914 = ORIENTED_EDGE ( 'NONE', *, *, #936, .F. ) ;
#21915 = CARTESIAN_POINT ( 'NONE',  ( 30.79999999999999716, -84.70000000000001705, 1.200000000000003064 ) ) ;
#21916 = CARTESIAN_POINT ( 'NONE',  ( -14.66174975910705136, -42.11054587065083155, 13.50000000000000000 ) ) ;
#21917 = DIRECTION ( 'NONE',  ( -0.000000000000000000, -1.000000000000000000, -0.000000000000000000 ) ) ;
#21918 = CARTESIAN_POINT ( 'NONE',  ( -3.627054932750481964, 32.61873716947361856, 42.50000000000000711 ) ) ;
#21919 = ADVANCED_FACE ( 'NONE', ( #16507 ), #5762, .T. ) ;
#21920 = DIRECTION ( 'NONE',  ( 0.000000000000000000, -0.000000000000000000, 1.000000000000000000 ) ) ;
#21921 = CARTESIAN_POINT ( 'NONE',  ( 9.641460742840918030, -32.11873716947361856, 68.50000000000000000 ) ) ;
#21922 = LINE ( 'NONE', #15414, #14581 ) ;
#21923 = CARTESIAN_POINT ( 'NONE',  ( -17.92752199202933738, -38.74634676501045760, 13.62426406871192874 ) ) ;
#21924 = CARTESIAN_POINT ( 'NONE',  ( -32.23382792203229741, 83.71979900898287497, 68.50000000000000000 ) ) ;
#21925 = ORIENTED_EDGE ( 'NONE', *, *, #18910, .T. ) ;
#21926 = DIRECTION ( 'NONE',  ( 0.000000000000000000, 0.000000000000000000, -1.000000000000000000 ) ) ;
#21927 = EDGE_CURVE ( 'NONE', #19115, #12570, #10405, .T. ) ;
#21928 = EDGE_CURVE ( 'NONE', #19413, #21087, #19769, .T. ) ;
#21929 = ORIENTED_EDGE ( 'NONE', *, *, #8939, .F. ) ;
#21930 = CARTESIAN_POINT ( 'NONE',  ( 14.66174975910705847, -51.76873716947361714, 13.50000000000000000 ) ) ;
#21931 = DIRECTION ( 'NONE',  ( 0.000000000000000000, 1.000000000000000000, 0.000000000000000000 ) ) ;
#21932 = VERTEX_POINT ( 'NONE', #9805 ) ;
#21933 = ORIENTED_EDGE ( 'NONE', *, *, #3683, .F. ) ;
#21934 = CARTESIAN_POINT ( 'NONE',  ( 14.96174975910705918, 51.86873716947361856, 14.00000000000000000 ) ) ;
#21935 = VERTEX_POINT ( 'NONE', #4664 ) ;
#21936 = EDGE_CURVE ( 'NONE', #20218, #12188, #9317, .T. ) ;
#21937 = DIRECTION ( 'NONE',  ( -0.000000000000000000, -1.000000000000000000, -0.000000000000000000 ) ) ;
#21938 = EDGE_LOOP ( 'NONE', ( #5615, #20444, #10060, #12871 ) ) ;
#21939 = DIRECTION ( 'NONE',  ( 1.000000000000000000, 0.000000000000000000, 0.000000000000000000 ) ) ;
#21940 = PRESENTATION_LAYER_ASSIGNMENT (  '', '', ( #20515 ) ) ;
#21941 = DIRECTION ( 'NONE',  ( 0.000000000000000000, -0.000000000000000000, -1.000000000000000000 ) ) ;
#21942 = DIRECTION ( 'NONE',  ( -0.2309407893632008379, 0.9729678061520339316, 3.204947270951672174E-15 ) ) ;
#21943 = CARTESIAN_POINT ( 'NONE',  ( -29.37540678000427619, 4.700000000000000178, 3.799999999999999822 ) ) ;
#21944 = DIRECTION ( 'NONE',  ( 0.000000000000000000, 1.000000000000000000, 0.000000000000000000 ) ) ;
#21945 = EDGE_CURVE ( 'NONE', #3260, #1513, #6485, .T. ) ;
#21946 = ADVANCED_FACE ( 'NONE', ( #9362 ), #18977, .T. ) ;
#21947 = AXIS2_PLACEMENT_3D ( 'NONE', #11136, #18064, #14379 ) ;
#21948 = LINE ( 'NONE', #16896, #11559 ) ;
#21949 = EDGE_CURVE ( 'NONE', #2108, #19696, #13026, .T. ) ;
#21950 = DIRECTION ( 'NONE',  ( -1.000000000000000000, 0.000000000000000000, 2.107255972849994642E-16 ) ) ;
#21951 = CARTESIAN_POINT ( 'NONE',  ( 0.000000000000000000, -5.000000000000000000, 7.500000000000000000 ) ) ;
#21952 = VERTEX_POINT ( 'NONE', #14719 ) ;
#21953 = CARTESIAN_POINT ( 'NONE',  ( 29.13662752439705272, 5.000000000000000000, 7.200000000000000178 ) ) ;
#21954 = EDGE_LOOP ( 'NONE', ( #13093, #9153, #16518, #13509 ) ) ;
#21955 = FACE_OUTER_BOUND ( 'NONE', #16414, .T. ) ;
#21956 = AXIS2_PLACEMENT_3D ( 'NONE', #18458, #6856, #18800 ) ;
#21957 = DIRECTION ( 'NONE',  ( -1.000000000000000000, 0.000000000000000000, 0.000000000000000000 ) ) ;
#21958 = ORIENTED_EDGE ( 'NONE', *, *, #20782, .T. ) ;
#21959 = AXIS2_PLACEMENT_3D ( 'NONE', #10027, #11684, #4989 ) ;
#21960 = ORIENTED_EDGE ( 'NONE', *, *, #19394, .T. ) ;
#21961 = DIRECTION ( 'NONE',  ( 0.000000000000000000, 1.000000000000000000, 0.000000000000000000 ) ) ;
#21962 = DIRECTION ( 'NONE',  ( 1.000000000000000000, 0.000000000000000000, 0.000000000000000000 ) ) ;
#21963 = ORIENTED_EDGE ( 'NONE', *, *, #4471, .F. ) ;
#21964 = EDGE_CURVE ( 'NONE', #1486, #2136, #18244, .T. ) ;
#21965 = ORIENTED_EDGE ( 'NONE', *, *, #18507, .F. ) ;
#21966 = ORIENTED_EDGE ( 'NONE', *, *, #15913, .F. ) ;
#21967 = DIRECTION ( 'NONE',  ( 0.000000000000000000, -0.000000000000000000, -1.000000000000000000 ) ) ;
#21968 = CYLINDRICAL_SURFACE ( 'NONE', #14536, 0.3000000000000016542 ) ;
#21969 = CARTESIAN_POINT ( 'NONE',  ( 1.724728116533979616, 42.31054587065082728, 31.80876104995653719 ) ) ;
#21970 = ORIENTED_EDGE ( 'NONE', *, *, #10874, .T. ) ;
#21971 = CARTESIAN_POINT ( 'NONE',  ( 30.49999999999999645, 70.00000000000000000, 10.00000000000000178 ) ) ;
#21972 = EDGE_CURVE ( 'NONE', #13239, #18812, #11454, .T. ) ;
#21973 = CARTESIAN_POINT ( 'NONE',  ( -23.36959064016851073, 45.26242829375641463, 68.50000000000000000 ) ) ;
#21974 = EDGE_CURVE ( 'NONE', #4912, #9883, #8932, .T. ) ;
#21975 = LINE ( 'NONE', #15358, #9343 ) ;
#21976 = CARTESIAN_POINT ( 'NONE',  ( 25.37540678000427263, -66.94634676501046044, 13.19999999999999929 ) ) ;
#21977 = ADVANCED_FACE ( 'NONE', ( #9704 ), #9590, .F. ) ;
#21978 = DIRECTION ( 'NONE',  ( 1.000000000000000000, 0.000000000000000000, 0.000000000000000000 ) ) ;
#21979 = ORIENTED_EDGE ( 'NONE', *, *, #17949, .T. ) ;
#21980 = ORIENTED_EDGE ( 'NONE', *, *, #6936, .F. ) ;
#21981 = ORIENTED_EDGE ( 'NONE', *, *, #18402, .T. ) ;
#21982 = CARTESIAN_POINT ( 'NONE',  ( -1.724728116533986721, 43.26054587065083012, 33.66679706732590915 ) ) ;
#21983 = DIRECTION ( 'NONE',  ( 1.000000000000000000, 0.000000000000000000, 0.000000000000000000 ) ) ;
#21984 = ORIENTED_EDGE ( 'NONE', *, *, #4148, .T. ) ;
#21985 = DIRECTION ( 'NONE',  ( 1.000000000000000000, -0.000000000000000000, -0.000000000000000000 ) ) ;
#21986 = AXIS2_PLACEMENT_3D ( 'NONE', #2594, #12864, #19384 ) ;
#21987 = EDGE_CURVE ( 'NONE', #1657, #4141, #841, .T. ) ;
#21988 = EDGE_LOOP ( 'NONE', ( #16465, #9009, #9977, #11174 ) ) ;
#21989 = DIRECTION ( 'NONE',  ( -0.000000000000000000, -0.000000000000000000, -1.000000000000000000 ) ) ;
#21990 = CARTESIAN_POINT ( 'NONE',  ( -15.95292532278785913, 52.11873716947361856, 68.00000000000000000 ) ) ;
#21991 = EDGE_CURVE ( 'NONE', #21652, #1033, #12811, .T. ) ;
#21992 = DIRECTION ( 'NONE',  ( 1.000000000000000000, 0.000000000000000000, 0.000000000000000000 ) ) ;
#21993 = DIRECTION ( 'NONE',  ( 0.000000000000000000, 0.000000000000000000, 1.000000000000000000 ) ) ;
#21994 = ORIENTED_EDGE ( 'NONE', *, *, #17890, .T. ) ;
#21995 = CARTESIAN_POINT ( 'NONE',  ( 1.724728116533979616, 42.36054587065083155, 27.80876104995653719 ) ) ;
#21996 = PLANE ( 'NONE',  #18183 ) ;
#21997 = CARTESIAN_POINT ( 'NONE',  ( -31.50000000000002132, 72.00000000000001421, 1.800000000000000044 ) ) ;
#21998 = CARTESIAN_POINT ( 'NONE',  ( 30.79999999999999716, -85.00000000000000000, 1.500000000000003997 ) ) ;
#21999 = ORIENTED_EDGE ( 'NONE', *, *, #20011, .T. ) ;
#22000 = CARTESIAN_POINT ( 'NONE',  ( 1.774728116533979438, 42.36054587065083155, 27.70876104995653577 ) ) ;
#22001 = CIRCLE ( 'NONE', #3415, 0.04999999999999991257 ) ;
#22002 = CIRCLE ( 'NONE', #5570, 0.1000000000000028644 ) ;
#22003 = EDGE_CURVE ( 'NONE', #689, #3262, #21444, .T. ) ;
#22004 = DIRECTION ( 'NONE',  ( 0.000000000000000000, 0.000000000000000000, -1.000000000000000000 ) ) ;
#22005 = VERTEX_POINT ( 'NONE', #17149 ) ;
#22006 = FACE_OUTER_BOUND ( 'NONE', #1137, .T. ) ;
#22007 = DIRECTION ( 'NONE',  ( 0.000000000000000000, 1.000000000000000000, 0.000000000000000000 ) ) ;
#22008 = VERTEX_POINT ( 'NONE', #18715 ) ;
#22009 = ORIENTED_EDGE ( 'NONE', *, *, #8033, .T. ) ;
#22010 = ORIENTED_EDGE ( 'NONE', *, *, #19576, .T. ) ;
#22011 = CYLINDRICAL_SURFACE ( 'NONE', #9546, 0.2999999999999999334 ) ;
#22012 = DIRECTION ( 'NONE',  ( 1.000000000000000000, 0.000000000000000000, 0.000000000000000000 ) ) ;
#22013 = ORIENTED_EDGE ( 'NONE', *, *, #12106, .T. ) ;
#22014 = AXIS2_PLACEMENT_3D ( 'NONE', #15673, #346, #19567 ) ;
#22015 = EDGE_LOOP ( 'NONE', ( #19881, #747, #7239, #11515 ) ) ;
#22016 = ORIENTED_EDGE ( 'NONE', *, *, #13604, .F. ) ;
#22017 = CARTESIAN_POINT ( 'NONE',  ( 31.50000000000002132, 71.00000000000001421, 1.500000000000000000 ) ) ;
#22018 = TOROIDAL_SURFACE ( 'NONE', #5588, 0.05000000000000000278, 0.05000000000000000278 ) ;
#22019 = AXIS2_PLACEMENT_3D ( 'NONE', #1278, #8346, #20107 ) ;
#22020 = TOROIDAL_SURFACE ( 'NONE', #1256, 5.300000000000004263, 0.2999999999999999889 ) ;
#22021 = EDGE_CURVE ( 'NONE', #4383, #8471, #10378, .T. ) ;
#22022 = ORIENTED_EDGE ( 'NONE', *, *, #12375, .T. ) ;
#22023 = CARTESIAN_POINT ( 'NONE',  ( -23.02398829872513986, -3.419159475692170158, 13.52813170334705184 ) ) ;
#22024 = ADVANCED_FACE ( 'NONE', ( #12105 ), #7154, .T. ) ;
#22025 = CARTESIAN_POINT ( 'NONE',  ( -15.21174975910705207, 52.11873716947361856, 68.00000000000000000 ) ) ;
#22026 = EDGE_CURVE ( 'NONE', #852, #483, #2485, .T. ) ;
#22027 = CARTESIAN_POINT ( 'NONE',  ( -8.638906393579159015, 43.51045099701597252, 68.06527860057354928 ) ) ;
#22028 = DIRECTION ( 'NONE',  ( -1.000000000000000000, -0.000000000000000000, -4.336808689942194441E-15 ) ) ;
#22029 = DIRECTION ( 'NONE',  ( 1.224646799147353207E-16, 0.000000000000000000, 1.000000000000000000 ) ) ;
#22030 = DIRECTION ( 'NONE',  ( -0.9729678061520319332, -0.2309407893632090258, 0.000000000000000000 ) ) ;
#22031 = CYLINDRICAL_SURFACE ( 'NONE', #5516, 0.2500000000000002220 ) ;
#22032 = CARTESIAN_POINT ( 'NONE',  ( 1.724728116533979616, 42.36054587065083155, 47.70876104995654288 ) ) ;
#22033 = VERTEX_POINT ( 'NONE', #12205 ) ;
#22034 = AXIS2_PLACEMENT_3D ( 'NONE', #15674, #17676, #557 ) ;
#22035 = TOROIDAL_SURFACE ( 'NONE', #12343, 3.750000000000000000, 1.250000000000000000 ) ;
#22036 = LINE ( 'NONE', #1431, #6993 ) ;
#22037 = AXIS2_PLACEMENT_3D ( 'NONE', #14091, #13762, #15459 ) ;
#22038 = DIRECTION ( 'NONE',  ( -1.000000000000000000, 0.000000000000000000, 0.000000000000000000 ) ) ;
#22039 = VERTEX_POINT ( 'NONE', #5523 ) ;
#22040 = CIRCLE ( 'NONE', #919, 0.2999999999999999334 ) ;
#22041 = CIRCLE ( 'NONE', #16641, 0.05000000000000143219 ) ;
#22042 = PLANE ( 'NONE',  #8887 ) ;
#22043 = CARTESIAN_POINT ( 'NONE',  ( -1.824728116533986810, 43.31054587065082728, 47.70876104995654288 ) ) ;
#22044 = ORIENTED_EDGE ( 'NONE', *, *, #20966, .T. ) ;
#22045 = ORIENTED_EDGE ( 'NONE', *, *, #3830, .F. ) ;
#22046 = CARTESIAN_POINT ( 'NONE',  ( -15.21174975910705207, 41.81054587065082728, 13.79999999999999893 ) ) ;
#22047 = ORIENTED_EDGE ( 'NONE', *, *, #11432, .T. ) ;
#22048 = CIRCLE ( 'NONE', #6683, 0.5000000000000004441 ) ;
#22049 = AXIS2_PLACEMENT_3D ( 'NONE', #16830, #3529, #11679 ) ;
#22050 = EDGE_CURVE ( 'NONE', #11165, #3327, #135, .T. ) ;
#22051 = DIRECTION ( 'NONE',  ( 0.000000000000000000, -1.000000000000000000, 0.000000000000000000 ) ) ;
#22052 = ORIENTED_EDGE ( 'NONE', *, *, #11911, .T. ) ;
#22053 = CARTESIAN_POINT ( 'NONE',  ( -29.42156627136959557, 2.562835948873662506, 0.09431749384236855216 ) ) ;
#22054 = AXIS2_PLACEMENT_3D ( 'NONE', #7887, #21304, #21537 ) ;
#22055 = DIRECTION ( 'NONE',  ( -3.491481338843133355E-15, 1.000000000000000000, 4.275831445896958607E-31 ) ) ;
#22056 = FACE_OUTER_BOUND ( 'NONE', #9037, .T. ) ;
#22057 = CARTESIAN_POINT ( 'NONE',  ( 14.71174975910707161, 51.61873716947361856, 68.50000000000000000 ) ) ;
#22058 = DIRECTION ( 'NONE',  ( 1.000000000000000000, -0.000000000000000000, 0.000000000000000000 ) ) ;
#22059 = DIRECTION ( 'NONE',  ( 0.000000000000000000, 0.000000000000000000, 1.000000000000000000 ) ) ;
#22060 = DIRECTION ( 'NONE',  ( 0.9823853469773031755, 0.1868663427273193067, 0.000000000000000000 ) ) ;
#22061 = AXIS2_PLACEMENT_3D ( 'NONE', #13472, #13358, #5202 ) ;
#22062 = CARTESIAN_POINT ( 'NONE',  ( -30.79999999999999361, -85.00000000000000000, 1.200000000000000622 ) ) ;
#22063 = DIRECTION ( 'NONE',  ( 1.000000000000000000, 0.000000000000000000, 0.000000000000000000 ) ) ;
#22064 = AXIS2_PLACEMENT_3D ( 'NONE', #3249, #16545, #6401 ) ;
#22065 = VECTOR ( 'NONE', #3981, 1000.000000000000000 ) ;
#22066 = VECTOR ( 'NONE', #20470, 1000.000000000000000 ) ;
#22067 = CARTESIAN_POINT ( 'NONE',  ( 31.50000000000002132, 72.00000000000001421, 3.500000000000000000 ) ) ;
#22068 = ORIENTED_EDGE ( 'NONE', *, *, #19465, .T. ) ;
#22069 = CARTESIAN_POINT ( 'NONE',  ( 27.37540678000427974, -5.683640910026986681, 42.50000000000000000 ) ) ;
#22070 = ORIENTED_EDGE ( 'NONE', *, *, #10992, .T. ) ;
#22071 = CIRCLE ( 'NONE', #14888, 0.3000000000000016542 ) ;
#22072 = VERTEX_POINT ( 'NONE', #3388 ) ;
#22073 = CYLINDRICAL_SURFACE ( 'NONE', #9589, 0.2999999999999999334 ) ;
#22074 = APPLICATION_PROTOCOL_DEFINITION ( 'draft international standard', 'automotive_design', 1998, #17584 ) ;
#22075 = EDGE_LOOP ( 'NONE', ( #14500, #13574, #18984, #21933 ) ) ;
#22076 = EDGE_LOOP ( 'NONE', ( #15294, #7784, #15246, #19636 ) ) ;
#22077 = ADVANCED_FACE ( 'NONE', ( #2147 ), #8981, .T. ) ;
#22078 = ORIENTED_EDGE ( 'NONE', *, *, #14548, .T. ) ;
#22079 = EDGE_CURVE ( 'NONE', #16679, #3824, #580, .T. ) ;
#22080 = CIRCLE ( 'NONE', #13843, 2.299999999999993161 ) ;
#22081 = TOROIDAL_SURFACE ( 'NONE', #19940, 1.750000000000000000, 0.2500000000000000000 ) ;
#22082 = PRODUCT_DEFINITION_CONTEXT ( 'detailed design', #15306, 'design' ) ;
#22083 = VERTEX_POINT ( 'NONE', #15468 ) ;
#22084 = CYLINDRICAL_SURFACE ( 'NONE', #651, 0.2999999999999999334 ) ;
#22085 = AXIS2_PLACEMENT_3D ( 'NONE', #5786, #8911, #10902 ) ;
#22086 = FACE_OUTER_BOUND ( 'NONE', #6090, .T. ) ;
#22087 = CARTESIAN_POINT ( 'NONE',  ( -17.45292532278785913, 38.74634676501045760, 13.99999999999999822 ) ) ;
#22088 = AXIS2_PLACEMENT_3D ( 'NONE', #17511, #11014, #19194 ) ;
#22089 = VERTEX_POINT ( 'NONE', #1921 ) ;
#22090 = CARTESIAN_POINT ( 'NONE',  ( -34.70000000000000284, -84.70000000000001705, 0.6000000000000033085 ) ) ;
#22091 = AXIS2_PLACEMENT_3D ( 'NONE', #5556, #11092, #17913 ) ;
#22092 = CARTESIAN_POINT ( 'NONE',  ( 23.32398829872514057, 3.528912754968628551, 13.79999999999999893 ) ) ;
#22093 = CARTESIAN_POINT ( 'NONE',  ( 0.000000000000000000, 0.000000000000000000, 42.50000000000000000 ) ) ;
#22094 = LINE ( 'NONE', #21762, #17709 ) ;
#22095 = ADVANCED_FACE ( 'NONE', ( #457 ), #11986, .T. ) ;
#22096 = DIRECTION ( 'NONE',  ( 0.000000000000000000, 1.000000000000000000, 0.000000000000000000 ) ) ;
#22097 = CIRCLE ( 'NONE', #2054, 0.2999999999999999334 ) ;
#22098 = ORIENTED_EDGE ( 'NONE', *, *, #781, .T. ) ;
#22099 = TOROIDAL_SURFACE ( 'NONE', #7822, 2.800000000000002043, 0.2999999999999999889 ) ;
#22100 = AXIS2_PLACEMENT_3D ( 'NONE', #7493, #2436, #7047 ) ;
#22101 = ORIENTED_EDGE ( 'NONE', *, *, #463, .T. ) ;
#22102 = VERTEX_POINT ( 'NONE', #6986 ) ;
#22103 = CYLINDRICAL_SURFACE ( 'NONE', #20646, 5.000000000000004441 ) ;
#22104 = FACE_OUTER_BOUND ( 'NONE', #913, .T. ) ;
#22105 = TOROIDAL_SURFACE ( 'NONE', #4235, 3.800000000000002931, 0.2999999999999999889 ) ;
#22106 = CARTESIAN_POINT ( 'NONE',  ( 15.21174975910705918, -52.10286008774954780, 13.87500000000000000 ) ) ;
#22107 = CIRCLE ( 'NONE', #11365, 0.5000000000000000000 ) ;
#22108 = TOROIDAL_SURFACE ( 'NONE', #8179, 1.500000000000000000, 0.5000000000000000000 ) ;
#22109 = ADVANCED_FACE ( 'NONE', ( #6886 ), #10543, .F. ) ;
#22110 = EDGE_CURVE ( 'NONE', #20083, #6358, #14283, .T. ) ;
#22111 = EDGE_CURVE ( 'NONE', #7135, #712, #13906, .T. ) ;
#22112 = VERTEX_POINT ( 'NONE', #7306 ) ;
#22113 = CARTESIAN_POINT ( 'NONE',  ( -21.92816239687475743, 42.46645089659918426, 68.25000000000000000 ) ) ;
#22114 = ADVANCED_FACE ( 'NONE', ( #5311 ), #3508, .F. ) ;
#22115 = FACE_OUTER_BOUND ( 'NONE', #19456, .T. ) ;
#22116 = AXIS2_PLACEMENT_3D ( 'NONE', #13181, #9617, #11502 ) ;
#22117 = DIRECTION ( 'NONE',  ( 0.000000000000000000, 0.000000000000000000, -1.000000000000000000 ) ) ;
#22118 = ORIENTED_EDGE ( 'NONE', *, *, #18340, .T. ) ;
#22119 = CARTESIAN_POINT ( 'NONE',  ( -1.824728116533986810, 42.36054587065083155, 41.71679706732590631 ) ) ;
#22120 = DIRECTION ( 'NONE',  ( 1.000000000000000000, 0.000000000000000000, 0.000000000000000000 ) ) ;
#22121 = DIRECTION ( 'NONE',  ( -0.9729678061520314891, -0.2309407893632107189, 0.000000000000000000 ) ) ;
#22122 = TOROIDAL_SURFACE ( 'NONE', #5692, 0.2999999999999999889, 0.2999999999999999889 ) ;
#22123 = DIRECTION ( 'NONE',  ( 1.000000000000000000, 0.000000000000000000, -2.388292521039847891E-16 ) ) ;
#22124 = FACE_OUTER_BOUND ( 'NONE', #9696, .T. ) ;
#22125 = ORIENTED_EDGE ( 'NONE', *, *, #18676, .T. ) ;
#22126 = DIRECTION ( 'NONE',  ( -0.000000000000000000, 1.000000000000000000, 0.000000000000000000 ) ) ;
#22127 = AXIS2_PLACEMENT_3D ( 'NONE', #18046, #19748, #5885 ) ;
#22128 = AXIS2_PLACEMENT_3D ( 'NONE', #13067, #19807, #21383 ) ;
#22129 = AXIS2_PLACEMENT_3D ( 'NONE', #15742, #20906, #9146 ) ;
#22130 = EDGE_CURVE ( 'NONE', #20601, #13526, #16775, .T. ) ;
#22131 = VERTEX_POINT ( 'NONE', #10341 ) ;
#22132 = DIRECTION ( 'NONE',  ( 0.000000000000000000, 0.000000000000000000, -1.000000000000000000 ) ) ;
#22133 = DIRECTION ( 'NONE',  ( 0.000000000000000000, 0.000000000000000000, 1.000000000000000000 ) ) ;
#22134 = DIRECTION ( 'NONE',  ( 0.000000000000000000, -1.000000000000000000, 0.000000000000000000 ) ) ;
#22135 = VERTEX_POINT ( 'NONE', #13890 ) ;
#22136 = VERTEX_POINT ( 'NONE', #19055 ) ;
#22137 = VERTEX_POINT ( 'NONE', #20064 ) ;
#22138 = CARTESIAN_POINT ( 'NONE',  ( 9.141460742840918030, 32.61873716947361856, 42.50000000000000711 ) ) ;
#22139 = SPHERICAL_SURFACE ( 'NONE', #8158, 0.2999999999999999889 ) ;
#22140 = CARTESIAN_POINT ( 'NONE',  ( 30.19999999999999574, 69.70000000000000284, 10.00000000000000178 ) ) ;
#22141 = AXIS2_PLACEMENT_3D ( 'NONE', #17201, #8715, #15512 ) ;
#22142 = ORIENTED_EDGE ( 'NONE', *, *, #9154, .T. ) ;
#22143 = EDGE_CURVE ( 'NONE', #13733, #18637, #4830, .T. ) ;
#22144 = ORIENTED_EDGE ( 'NONE', *, *, #15913, .T. ) ;
#22145 = FACE_OUTER_BOUND ( 'NONE', #12481, .T. ) ;
#22146 = EDGE_CURVE ( 'NONE', #847, #4394, #9871, .T. ) ;
#22147 = AXIS2_PLACEMENT_3D ( 'NONE', #3592, #3695, #12508 ) ;
#22148 = VERTEX_POINT ( 'NONE', #13223 ) ;
#22149 = CARTESIAN_POINT ( 'NONE',  ( -23.02398829872513986, -3.264788445950693507, 13.78841001078610873 ) ) ;
#22150 = DIRECTION ( 'NONE',  ( -1.000000000000000000, 0.000000000000000000, 0.000000000000000000 ) ) ;
#22151 = DIRECTION ( 'NONE',  ( 0.000000000000000000, 1.000000000000000000, -0.000000000000000000 ) ) ;
#22152 = LINE ( 'NONE', #12146, #18307 ) ;
#22153 = ORIENTED_EDGE ( 'NONE', *, *, #1382, .F. ) ;
#22154 = FACE_OUTER_BOUND ( 'NONE', #20633, .T. ) ;
#22155 = CARTESIAN_POINT ( 'NONE',  ( -25.37540678000427263, 67.54634676501045476, 7.500000000000000000 ) ) ;
#22156 = CARTESIAN_POINT ( 'NONE',  ( -18.05178606074127501, -38.87061083372239523, 13.49999999999999822 ) ) ;
#22157 = DIRECTION ( 'NONE',  ( 0.000000000000000000, 1.000000000000000000, 0.000000000000000000 ) ) ;
#22158 = ORIENTED_EDGE ( 'NONE', *, *, #17564, .T. ) ;
#22159 = LINE ( 'NONE', #8492, #1616 ) ;
#22160 = VECTOR ( 'NONE', #4031, 1000.000000000000000 ) ;
#22161 = VERTEX_POINT ( 'NONE', #14560 ) ;
#22162 = CARTESIAN_POINT ( 'NONE',  ( -15.21174975910705207, -51.86873716947361856, 14.00000000000000000 ) ) ;
#22163 = CARTESIAN_POINT ( 'NONE',  ( 1.824728116533979261, 42.36054587065083155, 27.70876104995653577 ) ) ;
#22164 = NEXT_ASSEMBLY_USAGE_OCCURRENCE ( 'NAUO1', ' ', ' ', #19031, #7141, $ ) ;
#22165 = NEXT_ASSEMBLY_USAGE_OCCURRENCE ( 'NAUO2', ' ', ' ', #19031, #2891, $ ) ;
#22166 = NEXT_ASSEMBLY_USAGE_OCCURRENCE ( 'NAUO3', ' ', ' ', #19031, #5212, $ ) ;
#22167 = NEXT_ASSEMBLY_USAGE_OCCURRENCE ( 'NAUO4', ' ', ' ', #19031, #19421, $ ) ;
#22168 = NEXT_ASSEMBLY_USAGE_OCCURRENCE ( 'NAUO5', ' ', ' ', #19031, #4251, $ ) ;
#22169 = NEXT_ASSEMBLY_USAGE_OCCURRENCE ( 'NAUO6', ' ', ' ', #19031, #16121, $ ) ;
#22170 = NEXT_ASSEMBLY_USAGE_OCCURRENCE ( 'NAUO7', ' ', ' ', #19031, #15053, $ ) ;
#22171 = NEXT_ASSEMBLY_USAGE_OCCURRENCE ( 'NAUO8', ' ', ' ', #19031, #7141, $ ) ;
#22172 = NEXT_ASSEMBLY_USAGE_OCCURRENCE ( 'NAUO9', ' ', ' ', #19031, #7141, $ ) ;
#22173 = NEXT_ASSEMBLY_USAGE_OCCURRENCE ( 'NAUO10', ' ', ' ', #19031, #7141, $ ) ;
#22174 = NEXT_ASSEMBLY_USAGE_OCCURRENCE ( 'NAUO11', ' ', ' ', #19031, #4251, $ ) ;
#22175 = NEXT_ASSEMBLY_USAGE_OCCURRENCE ( 'NAUO12', ' ', ' ', #19031, #4251, $ ) ;
#22176 = NEXT_ASSEMBLY_USAGE_OCCURRENCE ( 'NAUO13', ' ', ' ', #19031, #4251, $ ) ;
#22177 = NEXT_ASSEMBLY_USAGE_OCCURRENCE ( 'NAUO14', ' ', ' ', #19031, #15053, $ ) ;
#22178 = NEXT_ASSEMBLY_USAGE_OCCURRENCE ( 'NAUO15', ' ', ' ', #19031, #19421, $ ) ;
ENDSEC;
END-ISO-10303-21;
